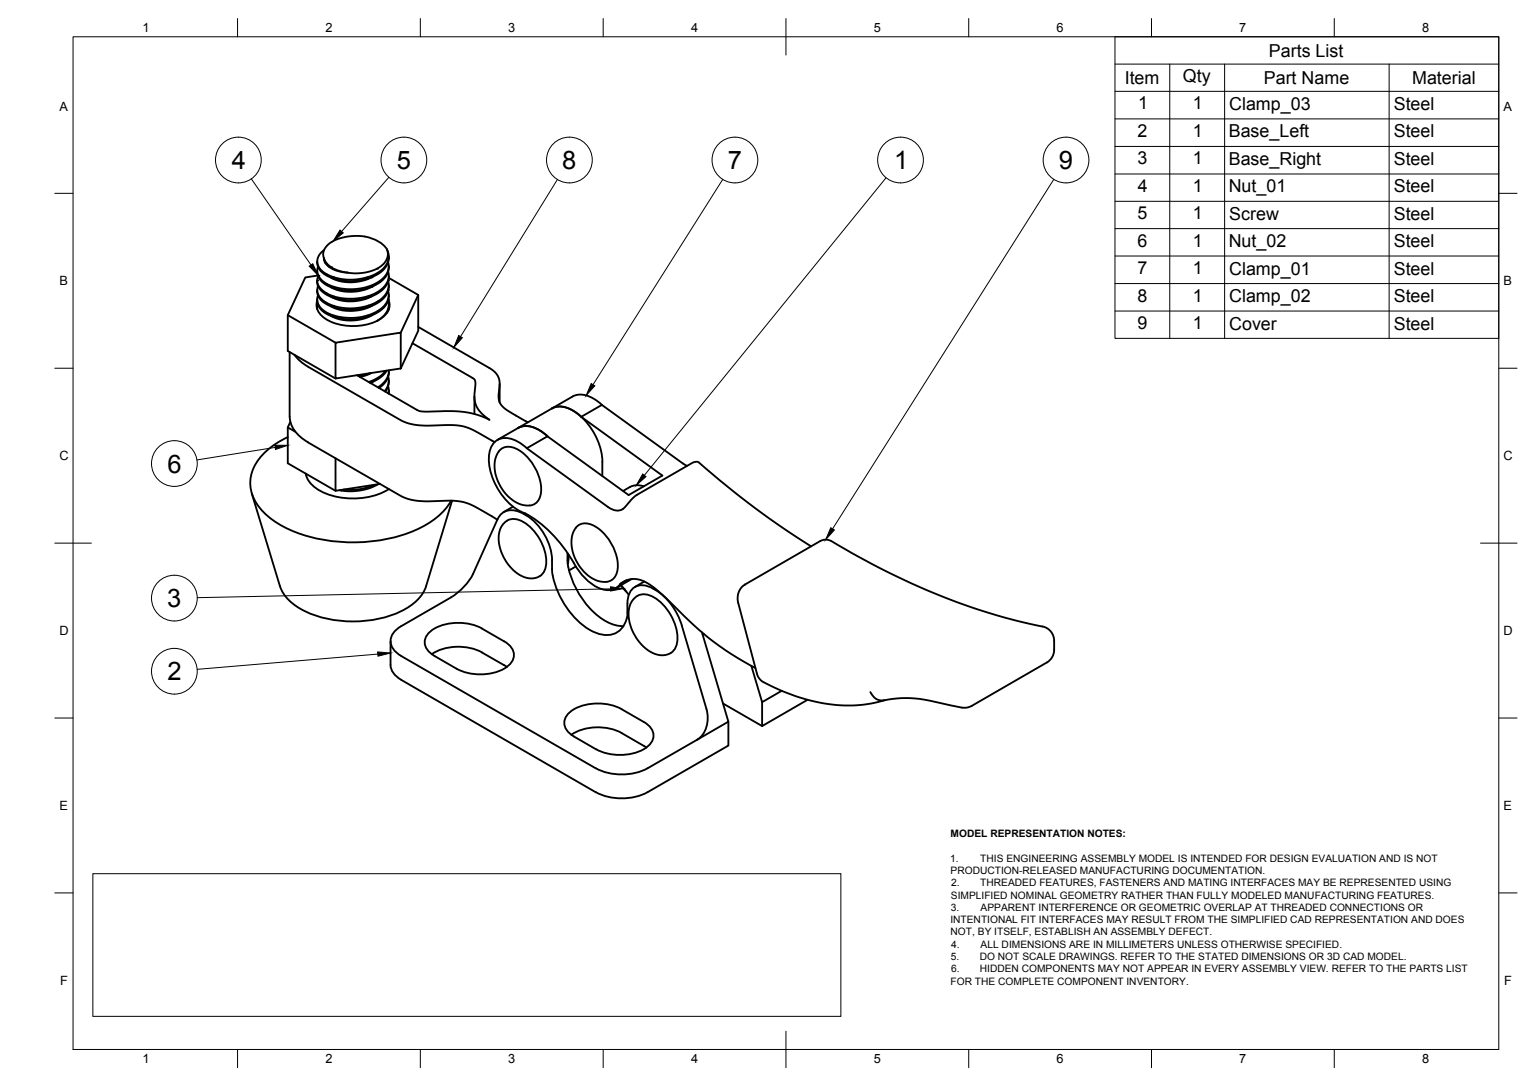
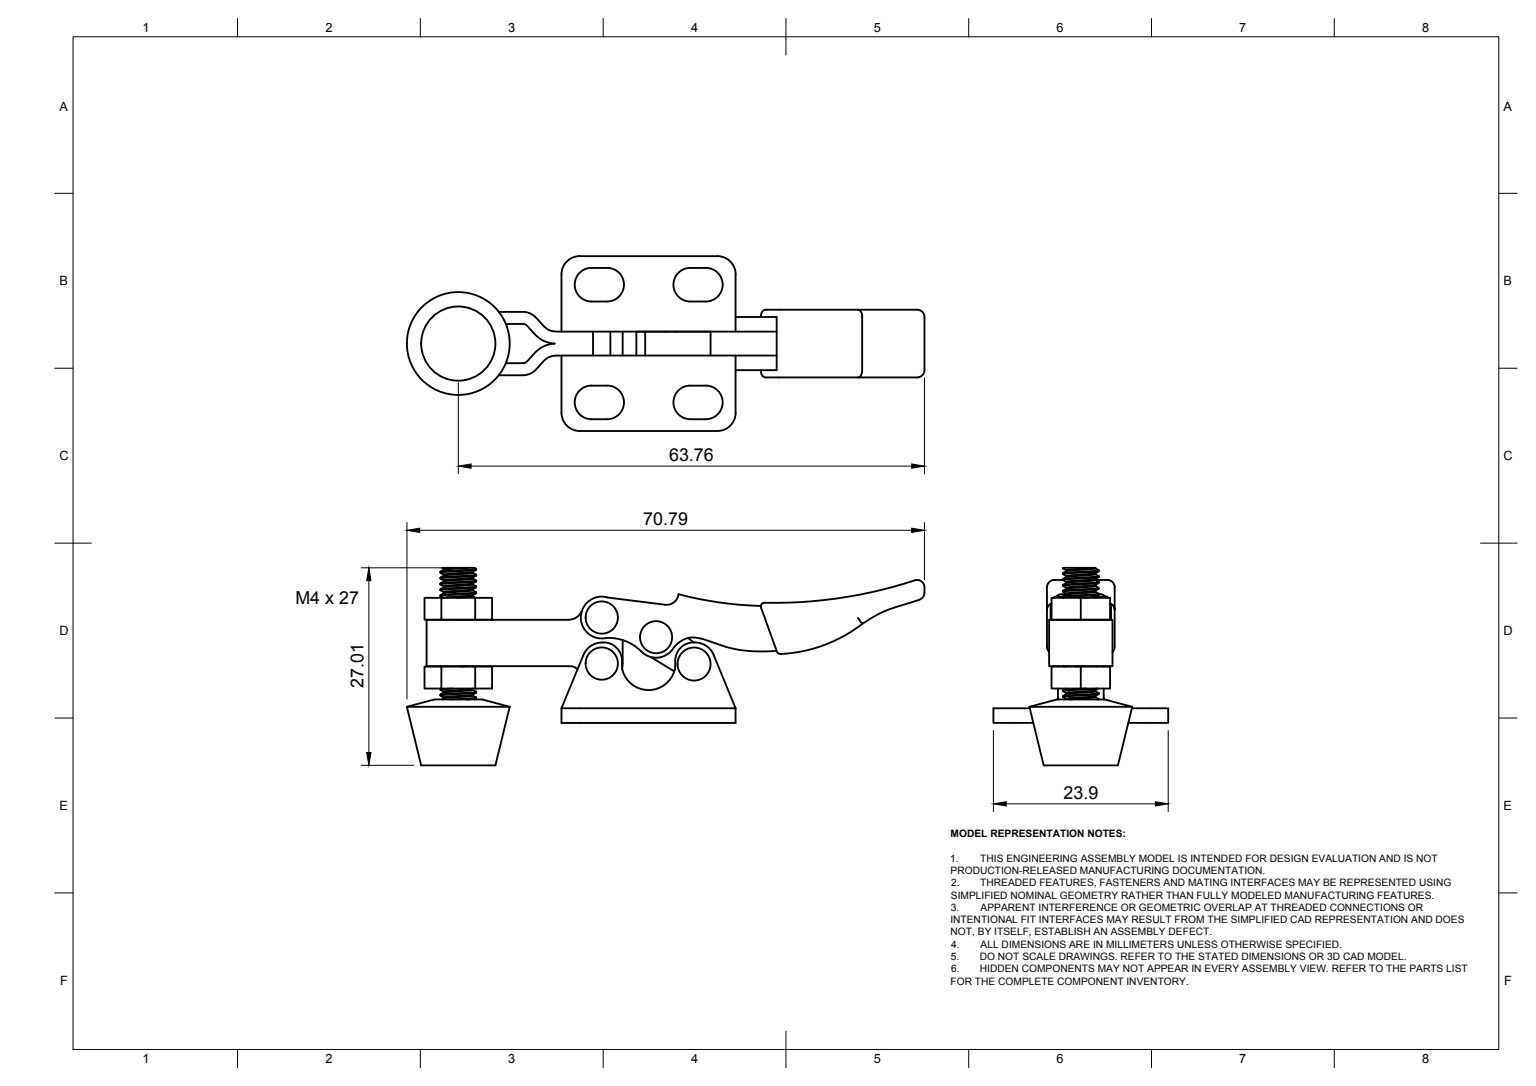
ISO-10303-21;
HEADER;
/* Generated by software containing ST-Developer
 * from STEP Tools, Inc. (www.steptools.com) 
 */

FILE_DESCRIPTION(
/* description */ (''),
/* implementation_level */ '2;1');

FILE_NAME(
/* name */ 'BR-203',
/* time_stamp */ '2026-10-05T16:20:14-07:00',
/* author */ (''),
/* organization */ (''),
/* preprocessor_version */ 'ST-DEVELOPER v20.2',
/* originating_system */ 'Autodesk Translation Framework v15.15.0.0',
/* authorisation */ '');

FILE_SCHEMA (('AUTOMOTIVE_DESIGN { 1 0 10303 214 3 1 1 }'));
ENDSEC;

DATA;
#10=MECHANICAL_DESIGN_GEOMETRIC_PRESENTATION_REPRESENTATION('',(#247,#248,
#249,#250,#251,#252,#253,#254,#255),#23577);
#11=ITEM_DEFINED_TRANSFORMATION($,$,#4267,#4665);
#12=ITEM_DEFINED_TRANSFORMATION($,$,#4284,#4666);
#13=ITEM_DEFINED_TRANSFORMATION($,$,#4354,#4667);
#14=ITEM_DEFINED_TRANSFORMATION($,$,#4424,#4668);
#15=ITEM_DEFINED_TRANSFORMATION($,$,#4436,#4669);
#16=ITEM_DEFINED_TRANSFORMATION($,$,#4473,#4670);
#17=ITEM_DEFINED_TRANSFORMATION($,$,#4485,#4671);
#18=ITEM_DEFINED_TRANSFORMATION($,$,#4573,#4672);
#19=ITEM_DEFINED_TRANSFORMATION($,$,#4607,#4673);
#20=(
REPRESENTATION_RELATIONSHIP($,$,#23612,#23611)
REPRESENTATION_RELATIONSHIP_WITH_TRANSFORMATION(#11)
SHAPE_REPRESENTATION_RELATIONSHIP()
);
#21=(
REPRESENTATION_RELATIONSHIP($,$,#23613,#23611)
REPRESENTATION_RELATIONSHIP_WITH_TRANSFORMATION(#12)
SHAPE_REPRESENTATION_RELATIONSHIP()
);
#22=(
REPRESENTATION_RELATIONSHIP($,$,#23614,#23611)
REPRESENTATION_RELATIONSHIP_WITH_TRANSFORMATION(#13)
SHAPE_REPRESENTATION_RELATIONSHIP()
);
#23=(
REPRESENTATION_RELATIONSHIP($,$,#23615,#23611)
REPRESENTATION_RELATIONSHIP_WITH_TRANSFORMATION(#14)
SHAPE_REPRESENTATION_RELATIONSHIP()
);
#24=(
REPRESENTATION_RELATIONSHIP($,$,#23616,#23611)
REPRESENTATION_RELATIONSHIP_WITH_TRANSFORMATION(#15)
SHAPE_REPRESENTATION_RELATIONSHIP()
);
#25=(
REPRESENTATION_RELATIONSHIP($,$,#23617,#23611)
REPRESENTATION_RELATIONSHIP_WITH_TRANSFORMATION(#16)
SHAPE_REPRESENTATION_RELATIONSHIP()
);
#26=(
REPRESENTATION_RELATIONSHIP($,$,#23618,#23611)
REPRESENTATION_RELATIONSHIP_WITH_TRANSFORMATION(#17)
SHAPE_REPRESENTATION_RELATIONSHIP()
);
#27=(
REPRESENTATION_RELATIONSHIP($,$,#23619,#23611)
REPRESENTATION_RELATIONSHIP_WITH_TRANSFORMATION(#18)
SHAPE_REPRESENTATION_RELATIONSHIP()
);
#28=(
REPRESENTATION_RELATIONSHIP($,$,#23620,#23611)
REPRESENTATION_RELATIONSHIP_WITH_TRANSFORMATION(#19)
SHAPE_REPRESENTATION_RELATIONSHIP()
);
#29=CONTEXT_DEPENDENT_SHAPE_REPRESENTATION(#20,#23602);
#30=CONTEXT_DEPENDENT_SHAPE_REPRESENTATION(#21,#23603);
#31=CONTEXT_DEPENDENT_SHAPE_REPRESENTATION(#22,#23604);
#32=CONTEXT_DEPENDENT_SHAPE_REPRESENTATION(#23,#23605);
#33=CONTEXT_DEPENDENT_SHAPE_REPRESENTATION(#24,#23606);
#34=CONTEXT_DEPENDENT_SHAPE_REPRESENTATION(#25,#23607);
#35=CONTEXT_DEPENDENT_SHAPE_REPRESENTATION(#26,#23608);
#36=CONTEXT_DEPENDENT_SHAPE_REPRESENTATION(#27,#23609);
#37=CONTEXT_DEPENDENT_SHAPE_REPRESENTATION(#28,#23610);
#38=NEXT_ASSEMBLY_USAGE_OCCURRENCE('Clamp_03:1','Clamp_03:1',
'Clamp_03:1',#23622,#23623,'Clamp_03:1');
#39=NEXT_ASSEMBLY_USAGE_OCCURRENCE('Base_Left:1','Base_Left:1',
'Base_Left:1',#23622,#23624,'Base_Left:1');
#40=NEXT_ASSEMBLY_USAGE_OCCURRENCE('Base_Right:1','Base_Right:1',
'Base_Right:1',#23622,#23625,'Base_Right:1');
#41=NEXT_ASSEMBLY_USAGE_OCCURRENCE('Nut_01:1','Nut_01:1','Nut_01:1',#23622,
#23626,'Nut_01:1');
#42=NEXT_ASSEMBLY_USAGE_OCCURRENCE('Screw:1','Screw:1','Screw:1',#23622,
#23627,'Screw:1');
#43=NEXT_ASSEMBLY_USAGE_OCCURRENCE('Nut_02:1','Nut_02:1','Nut_02:1',#23622,
#23628,'Nut_02:1');
#44=NEXT_ASSEMBLY_USAGE_OCCURRENCE('Clamp_01:1','Clamp_01:1',
'Clamp_01:1',#23622,#23629,'Clamp_01:1');
#45=NEXT_ASSEMBLY_USAGE_OCCURRENCE('Clamp_02:1','Clamp_02:1',
'Clamp_02:1',#23622,#23630,'Clamp_02:1');
#46=NEXT_ASSEMBLY_USAGE_OCCURRENCE('Cover:1','Cover:1','Cover:1',#23622,
#23631,'Cover:1');
#47=SPHERICAL_SURFACE('',#4635,1.);
#48=SPHERICAL_SURFACE('',#4644,1.);
#49=SPHERICAL_SURFACE('',#4650,1.);
#50=SPHERICAL_SURFACE('',#4654,1.);
#51=CONICAL_SURFACE('',#4468,5.14028464662889,1.31156275926766);
#52=CONICAL_SURFACE('',#4470,6.05319927020769,0.239535482048054);
#53=B_SPLINE_SURFACE_WITH_KNOTS('',3,3,((#19950,#19951,#19952,#19953,#19954,
#19955,#19956,#19957,#19958,#19959,#19960,#19961,#19962,#19963,#19964,#19965,
#19966,#19967,#19968,#19969,#19970,#19971,#19972,#19973,#19974,#19975,#19976,
#19977,#19978,#19979,#19980,#19981,#19982,#19983,#19984,#19985,#19986,#19987,
#19988,#19989,#19990,#19991,#19992,#19993,#19994,#19995,#19996,#19997,#19998,
#19999,#20000,#20001,#20002,#20003,#20004,#20005,#20006,#20007,#20008,#20009,
#20010,#20011,#20012,#20013,#20014,#20015,#20016,#20017,#20018,#20019,#20020,
#20021,#20022,#20023,#20024,#20025,#20026,#20027,#20028,#20029,#20030,#20031,
#20032,#20033,#20034,#20035,#20036,#20037,#20038,#20039,#20040,#20041,#20042,
#20043,#20044,#20045,#20046,#20047,#20048,#20049,#20050,#20051,#20052,#20053,
#20054,#20055,#20056,#20057,#20058,#20059,#20060,#20061,#20062,#20063,#20064,
#20065,#20066,#20067,#20068,#20069,#20070,#20071,#20072,#20073,#20074,#20075,
#20076,#20077,#20078,#20079,#20080,#20081,#20082,#20083,#20084,#20085,#20086,
#20087,#20088,#20089,#20090,#20091,#20092,#20093,#20094,#20095,#20096),
(#20097,#20098,#20099,#20100,#20101,#20102,#20103,#20104,#20105,#20106,
#20107,#20108,#20109,#20110,#20111,#20112,#20113,#20114,#20115,#20116,#20117,
#20118,#20119,#20120,#20121,#20122,#20123,#20124,#20125,#20126,#20127,#20128,
#20129,#20130,#20131,#20132,#20133,#20134,#20135,#20136,#20137,#20138,#20139,
#20140,#20141,#20142,#20143,#20144,#20145,#20146,#20147,#20148,#20149,#20150,
#20151,#20152,#20153,#20154,#20155,#20156,#20157,#20158,#20159,#20160,#20161,
#20162,#20163,#20164,#20165,#20166,#20167,#20168,#20169,#20170,#20171,#20172,
#20173,#20174,#20175,#20176,#20177,#20178,#20179,#20180,#20181,#20182,#20183,
#20184,#20185,#20186,#20187,#20188,#20189,#20190,#20191,#20192,#20193,#20194,
#20195,#20196,#20197,#20198,#20199,#20200,#20201,#20202,#20203,#20204,#20205,
#20206,#20207,#20208,#20209,#20210,#20211,#20212,#20213,#20214,#20215,#20216,
#20217,#20218,#20219,#20220,#20221,#20222,#20223,#20224,#20225,#20226,#20227,
#20228,#20229,#20230,#20231,#20232,#20233,#20234,#20235,#20236,#20237,#20238,
#20239,#20240,#20241,#20242,#20243),(#20244,#20245,#20246,#20247,#20248,
#20249,#20250,#20251,#20252,#20253,#20254,#20255,#20256,#20257,#20258,#20259,
#20260,#20261,#20262,#20263,#20264,#20265,#20266,#20267,#20268,#20269,#20270,
#20271,#20272,#20273,#20274,#20275,#20276,#20277,#20278,#20279,#20280,#20281,
#20282,#20283,#20284,#20285,#20286,#20287,#20288,#20289,#20290,#20291,#20292,
#20293,#20294,#20295,#20296,#20297,#20298,#20299,#20300,#20301,#20302,#20303,
#20304,#20305,#20306,#20307,#20308,#20309,#20310,#20311,#20312,#20313,#20314,
#20315,#20316,#20317,#20318,#20319,#20320,#20321,#20322,#20323,#20324,#20325,
#20326,#20327,#20328,#20329,#20330,#20331,#20332,#20333,#20334,#20335,#20336,
#20337,#20338,#20339,#20340,#20341,#20342,#20343,#20344,#20345,#20346,#20347,
#20348,#20349,#20350,#20351,#20352,#20353,#20354,#20355,#20356,#20357,#20358,
#20359,#20360,#20361,#20362,#20363,#20364,#20365,#20366,#20367,#20368,#20369,
#20370,#20371,#20372,#20373,#20374,#20375,#20376,#20377,#20378,#20379,#20380,
#20381,#20382,#20383,#20384,#20385,#20386,#20387,#20388,#20389,#20390),
(#20391,#20392,#20393,#20394,#20395,#20396,#20397,#20398,#20399,#20400,
#20401,#20402,#20403,#20404,#20405,#20406,#20407,#20408,#20409,#20410,#20411,
#20412,#20413,#20414,#20415,#20416,#20417,#20418,#20419,#20420,#20421,#20422,
#20423,#20424,#20425,#20426,#20427,#20428,#20429,#20430,#20431,#20432,#20433,
#20434,#20435,#20436,#20437,#20438,#20439,#20440,#20441,#20442,#20443,#20444,
#20445,#20446,#20447,#20448,#20449,#20450,#20451,#20452,#20453,#20454,#20455,
#20456,#20457,#20458,#20459,#20460,#20461,#20462,#20463,#20464,#20465,#20466,
#20467,#20468,#20469,#20470,#20471,#20472,#20473,#20474,#20475,#20476,#20477,
#20478,#20479,#20480,#20481,#20482,#20483,#20484,#20485,#20486,#20487,#20488,
#20489,#20490,#20491,#20492,#20493,#20494,#20495,#20496,#20497,#20498,#20499,
#20500,#20501,#20502,#20503,#20504,#20505,#20506,#20507,#20508,#20509,#20510,
#20511,#20512,#20513,#20514,#20515,#20516,#20517,#20518,#20519,#20520,#20521,
#20522,#20523,#20524,#20525,#20526,#20527,#20528,#20529,#20530,#20531,#20532,
#20533,#20534,#20535,#20536,#20537)),.UNSPECIFIED.,.F.,.F.,.F.,(4,4),(4,
1,1,1,1,1,1,1,1,1,1,1,1,1,1,1,1,1,1,1,1,1,1,1,1,1,1,1,1,1,1,1,1,1,1,1,1,
1,1,1,1,1,1,1,1,1,1,1,1,1,1,1,1,1,1,1,1,1,1,1,1,1,1,1,1,1,1,1,1,1,1,1,1,
1,1,1,1,1,1,1,1,1,1,1,1,1,1,1,1,1,1,1,1,1,1,1,1,1,1,1,1,1,1,1,1,1,1,1,1,
1,1,1,1,1,1,1,1,1,1,1,1,1,1,1,1,1,1,1,1,1,1,1,1,1,1,1,1,1,1,1,1,1,1,1,4),
(-0.000407634560164902,0.0529903850324167),(8.30815772716265,9.30425680398324,
10.3003558808038,11.2964549576244,12.292554034445,13.2886531112656,14.2847521880862,
15.2808512649068,16.2769503417274,17.273049418548,18.2691484953686,19.2652475721892,
20.2613466490097,21.2574457258303,22.2535448026509,23.2496438794715,24.2457429562921,
25.2418420331127,26.2379411099333,27.2340401867539,28.2301392635745,29.2262383403951,
30.2223374172156,31.2184364940362,32.2145355708568,33.2106346476774,34.206733724498,
35.2028328013186,36.1989318781392,37.1950309549598,38.1911300317804,39.187229108601,
40.1833281854216,41.1794272622421,42.1755263390627,43.1716254158833,44.1677244927039,
45.1638235695245,46.1599226463451,47.1560217231657,48.1521207999863,49.1482198768069,
50.1443189536275,51.1404180304481,52.1365171072686,53.1326161840892,54.1287152609098,
55.1248143377304,56.120913414551,57.1170124913716,58.1131115681922,59.1092106450128,
60.1053097218334,61.101408798654,62.0975078754745,63.0936069522951,64.0897060291157,
65.0858051059363,66.0819041827569,67.0780032595775,68.0741023363981,69.0702014132187,
70.0663004900393,71.0623995668599,72.0584986436805,73.0545977205011,74.0506967973216,
75.0467958741422,76.0428949509628,77.0389940277834,78.035093104604,79.0311921814246,
80.0272912582452,81.0233903350658,82.0194894118864,83.015588488707,84.0116875655276,
85.0077866423481,86.0038857191687,86.9999847959893,87.9960838728099,88.9921829496305,
89.9882820264511,90.9843811032717,91.9804801800923,92.9765792569129,93.9726783337335,
94.968777410554,95.9648764873746,96.9609755641952,97.9570746410158,98.9531737178364,
99.949272794657,100.945371871478,101.941470948298,102.937570025119,103.933669101939,
104.92976817876,105.925867255581,106.921966332401,107.918065409222,108.914164486042,
109.910263562863,110.906362639683,111.902461716504,112.898560793325,113.894659870145,
114.890758946966,115.886858023786,116.882957100607,117.879056177428,118.875155254248,
119.871254331069,120.867353407889,121.86345248471,122.859551561531,123.855650638351,
124.851749715172,125.847848791992,126.843947868813,127.840046945634,128.836146022454,
129.832245099275,130.828344176095,131.824443252916,132.820542329736,133.816641406557,
134.812740483378,135.808839560198,136.804938637019,137.801037713839,138.79713679066,
139.793235867481,140.789334944301,141.785434021122,142.781533097942,143.777632174763,
144.773731251584,145.769830328404,146.765929405225,147.762028482045,148.758127558866,
149.754226635687,150.750325712507,151.746832423888),.UNSPECIFIED.);
#54=B_SPLINE_SURFACE_WITH_KNOTS('',3,3,((#20716,#20717,#20718,#20719,#20720,
#20721,#20722,#20723,#20724,#20725,#20726,#20727,#20728,#20729,#20730,#20731,
#20732,#20733,#20734,#20735,#20736,#20737,#20738,#20739,#20740,#20741,#20742,
#20743,#20744,#20745,#20746,#20747,#20748,#20749,#20750,#20751,#20752,#20753,
#20754,#20755,#20756,#20757,#20758,#20759,#20760,#20761,#20762,#20763,#20764,
#20765,#20766,#20767,#20768,#20769,#20770,#20771,#20772,#20773,#20774,#20775,
#20776,#20777,#20778,#20779,#20780,#20781,#20782,#20783,#20784,#20785,#20786,
#20787,#20788,#20789,#20790,#20791,#20792,#20793,#20794,#20795,#20796,#20797,
#20798,#20799,#20800,#20801,#20802,#20803,#20804,#20805,#20806,#20807,#20808,
#20809,#20810,#20811,#20812,#20813,#20814,#20815,#20816,#20817,#20818,#20819,
#20820,#20821,#20822,#20823,#20824,#20825,#20826,#20827,#20828,#20829,#20830,
#20831,#20832,#20833,#20834,#20835,#20836,#20837,#20838,#20839,#20840,#20841,
#20842,#20843,#20844,#20845,#20846,#20847,#20848,#20849,#20850,#20851,#20852,
#20853,#20854,#20855,#20856,#20857,#20858,#20859,#20860,#20861,#20862),
(#20863,#20864,#20865,#20866,#20867,#20868,#20869,#20870,#20871,#20872,
#20873,#20874,#20875,#20876,#20877,#20878,#20879,#20880,#20881,#20882,#20883,
#20884,#20885,#20886,#20887,#20888,#20889,#20890,#20891,#20892,#20893,#20894,
#20895,#20896,#20897,#20898,#20899,#20900,#20901,#20902,#20903,#20904,#20905,
#20906,#20907,#20908,#20909,#20910,#20911,#20912,#20913,#20914,#20915,#20916,
#20917,#20918,#20919,#20920,#20921,#20922,#20923,#20924,#20925,#20926,#20927,
#20928,#20929,#20930,#20931,#20932,#20933,#20934,#20935,#20936,#20937,#20938,
#20939,#20940,#20941,#20942,#20943,#20944,#20945,#20946,#20947,#20948,#20949,
#20950,#20951,#20952,#20953,#20954,#20955,#20956,#20957,#20958,#20959,#20960,
#20961,#20962,#20963,#20964,#20965,#20966,#20967,#20968,#20969,#20970,#20971,
#20972,#20973,#20974,#20975,#20976,#20977,#20978,#20979,#20980,#20981,#20982,
#20983,#20984,#20985,#20986,#20987,#20988,#20989,#20990,#20991,#20992,#20993,
#20994,#20995,#20996,#20997,#20998,#20999,#21000,#21001,#21002,#21003,#21004,
#21005,#21006,#21007,#21008,#21009),(#21010,#21011,#21012,#21013,#21014,
#21015,#21016,#21017,#21018,#21019,#21020,#21021,#21022,#21023,#21024,#21025,
#21026,#21027,#21028,#21029,#21030,#21031,#21032,#21033,#21034,#21035,#21036,
#21037,#21038,#21039,#21040,#21041,#21042,#21043,#21044,#21045,#21046,#21047,
#21048,#21049,#21050,#21051,#21052,#21053,#21054,#21055,#21056,#21057,#21058,
#21059,#21060,#21061,#21062,#21063,#21064,#21065,#21066,#21067,#21068,#21069,
#21070,#21071,#21072,#21073,#21074,#21075,#21076,#21077,#21078,#21079,#21080,
#21081,#21082,#21083,#21084,#21085,#21086,#21087,#21088,#21089,#21090,#21091,
#21092,#21093,#21094,#21095,#21096,#21097,#21098,#21099,#21100,#21101,#21102,
#21103,#21104,#21105,#21106,#21107,#21108,#21109,#21110,#21111,#21112,#21113,
#21114,#21115,#21116,#21117,#21118,#21119,#21120,#21121,#21122,#21123,#21124,
#21125,#21126,#21127,#21128,#21129,#21130,#21131,#21132,#21133,#21134,#21135,
#21136,#21137,#21138,#21139,#21140,#21141,#21142,#21143,#21144,#21145,#21146,
#21147,#21148,#21149,#21150,#21151,#21152,#21153,#21154,#21155,#21156),
(#21157,#21158,#21159,#21160,#21161,#21162,#21163,#21164,#21165,#21166,
#21167,#21168,#21169,#21170,#21171,#21172,#21173,#21174,#21175,#21176,#21177,
#21178,#21179,#21180,#21181,#21182,#21183,#21184,#21185,#21186,#21187,#21188,
#21189,#21190,#21191,#21192,#21193,#21194,#21195,#21196,#21197,#21198,#21199,
#21200,#21201,#21202,#21203,#21204,#21205,#21206,#21207,#21208,#21209,#21210,
#21211,#21212,#21213,#21214,#21215,#21216,#21217,#21218,#21219,#21220,#21221,
#21222,#21223,#21224,#21225,#21226,#21227,#21228,#21229,#21230,#21231,#21232,
#21233,#21234,#21235,#21236,#21237,#21238,#21239,#21240,#21241,#21242,#21243,
#21244,#21245,#21246,#21247,#21248,#21249,#21250,#21251,#21252,#21253,#21254,
#21255,#21256,#21257,#21258,#21259,#21260,#21261,#21262,#21263,#21264,#21265,
#21266,#21267,#21268,#21269,#21270,#21271,#21272,#21273,#21274,#21275,#21276,
#21277,#21278,#21279,#21280,#21281,#21282,#21283,#21284,#21285,#21286,#21287,
#21288,#21289,#21290,#21291,#21292,#21293,#21294,#21295,#21296,#21297,#21298,
#21299,#21300,#21301,#21302,#21303)),.UNSPECIFIED.,.F.,.F.,.F.,(4,4),(4,
1,1,1,1,1,1,1,1,1,1,1,1,1,1,1,1,1,1,1,1,1,1,1,1,1,1,1,1,1,1,1,1,1,1,1,1,
1,1,1,1,1,1,1,1,1,1,1,1,1,1,1,1,1,1,1,1,1,1,1,1,1,1,1,1,1,1,1,1,1,1,1,1,
1,1,1,1,1,1,1,1,1,1,1,1,1,1,1,1,1,1,1,1,1,1,1,1,1,1,1,1,1,1,1,1,1,1,1,1,
1,1,1,1,1,1,1,1,1,1,1,1,1,1,1,1,1,1,1,1,1,1,1,1,1,1,1,1,1,1,1,1,1,1,1,4),
(-0.000364909195550823,0.0530331194684996),(11.6159855549096,12.6124922741621,
13.6085913509826,14.6046904278032,15.6007895046238,16.5968885814444,17.592987658265,
18.5890867350856,19.5851858119062,20.5812848887268,21.5773839655474,22.573483042368,
23.5695821191886,24.5656811960091,25.5617802728297,26.5578793496503,27.5539784264709,
28.5500775032915,29.5461765801121,30.5422756569327,31.5383747337533,32.5344738105739,
33.5305728873945,34.5266719642151,35.5227710410356,36.5188701178562,37.5149691946768,
38.5110682714974,39.507167348318,40.5032664251386,41.4993655019592,42.4954645787798,
43.4915636556004,44.487662732421,45.4837618092415,46.4798608860621,47.4759599628827,
48.4720590397033,49.4681581165239,50.4642571933445,51.4603562701651,52.4564553469857,
53.4525544238063,54.4486535006269,55.4447525774475,56.4408516542681,57.4369507310886,
58.4330498079092,59.4291488847298,60.4252479615504,61.421347038371,62.4174461151916,
63.4135451920122,64.4096442688328,65.4057433456534,66.4018424224739,67.3979414992945,
68.3940405761151,69.3901396529357,70.3862387297563,71.3823378065769,72.3784368833975,
73.3745359602181,74.3706350370387,75.3667341138593,76.3628331906799,77.3589322675004,
78.355031344321,79.3511304211416,80.3472294979622,81.3433285747828,82.3394276516034,
83.335526728424,84.3316258052446,85.3277248820652,86.3238239588858,87.3199230357064,
88.316022112527,89.3121211893476,90.3082202661681,91.3043193429887,92.3004184198093,
93.2965174966299,94.2926165734505,95.2887156502711,96.2848147270917,97.2809138039123,
98.2770128807329,99.2731119575535,100.269211034374,101.265310111195,102.261409188015,
103.257508264836,104.253607341656,105.249706418477,106.245805495298,107.241904572118,
108.238003648939,109.234102725759,110.23020180258,111.226300879401,112.222399956221,
113.218499033042,114.214598109862,115.210697186683,116.206796263503,117.202895340324,
118.198994417145,119.195093493965,120.191192570786,121.187291647606,122.183390724427,
123.179489801248,124.175588878068,125.171687954889,126.167787031709,127.16388610853,
128.159985185351,129.156084262171,130.152183338992,131.148282415812,132.144381492633,
133.140480569454,134.136579646274,135.132678723095,136.128777799915,137.124876876736,
138.120975953556,139.117075030377,140.113174107198,141.109273184018,142.105372260839,
143.101471337659,144.09757041448,145.093669491301,146.089768568121,147.085867644942,
148.081966721762,149.078065798583,150.074164875404,151.070263952224,152.066363029045,
153.062462105865,154.058561182686,155.054660259507),.UNSPECIFIED.);
#55=B_SPLINE_SURFACE_WITH_KNOTS('',5,1,((#21755,#21756),(#21757,#21758),
(#21759,#21760),(#21761,#21762),(#21763,#21764),(#21765,#21766),(#21767,
#21768),(#21769,#21770),(#21771,#21772),(#21773,#21774),(#21775,#21776),
(#21777,#21778),(#21779,#21780),(#21781,#21782),(#21783,#21784),(#21785,
#21786),(#21787,#21788),(#21789,#21790),(#21791,#21792),(#21793,#21794),
(#21795,#21796),(#21797,#21798),(#21799,#21800),(#21801,#21802),(#21803,
#21804),(#21805,#21806),(#21807,#21808),(#21809,#21810),(#21811,#21812),
(#21813,#21814),(#21815,#21816),(#21817,#21818),(#21819,#21820),(#21821,
#21822),(#21823,#21824),(#21825,#21826),(#21827,#21828),(#21829,#21830),
(#21831,#21832),(#21833,#21834),(#21835,#21836),(#21837,#21838),(#21839,
#21840),(#21841,#21842),(#21843,#21844),(#21845,#21846),(#21847,#21848),
(#21849,#21850),(#21851,#21852),(#21853,#21854),(#21855,#21856),(#21857,
#21858),(#21859,#21860),(#21861,#21862),(#21863,#21864)),.UNSPECIFIED.,
 .F.,.F.,.F.,(6,1,1,1,1,1,1,1,1,1,1,1,1,1,1,1,1,1,1,1,1,1,1,1,1,1,1,1,1,
1,1,1,1,1,1,1,1,1,1,1,1,1,1,1,1,1,1,1,1,1,6),(2,2),(0.,0.02,0.04,0.06,0.08,
0.1,0.12,0.14,0.16,0.18,0.2,0.22,0.24,0.26,0.28,0.3,0.32,0.34,0.36,0.38,
0.4,0.42,0.44,0.46,0.48,0.5,0.52,0.54,0.56,0.58,0.6,0.62,0.64,0.66,0.68,
0.7,0.72,0.74,0.76,0.78,0.8,0.82,0.84,0.86,0.88,0.9,0.92,0.940000000000001,
0.960000000000001,0.980000000000001,0.99866513431215),(0.,0.24),
 .UNSPECIFIED.);
#56=B_SPLINE_SURFACE_WITH_KNOTS('',5,1,((#22096,#22097),(#22098,#22099),
(#22100,#22101),(#22102,#22103),(#22104,#22105),(#22106,#22107),(#22108,
#22109),(#22110,#22111),(#22112,#22113),(#22114,#22115),(#22116,#22117),
(#22118,#22119),(#22120,#22121),(#22122,#22123),(#22124,#22125),(#22126,
#22127),(#22128,#22129),(#22130,#22131),(#22132,#22133),(#22134,#22135),
(#22136,#22137),(#22138,#22139),(#22140,#22141),(#22142,#22143),(#22144,
#22145),(#22146,#22147),(#22148,#22149),(#22150,#22151),(#22152,#22153),
(#22154,#22155),(#22156,#22157),(#22158,#22159),(#22160,#22161),(#22162,
#22163),(#22164,#22165),(#22166,#22167),(#22168,#22169),(#22170,#22171),
(#22172,#22173),(#22174,#22175),(#22176,#22177),(#22178,#22179),(#22180,
#22181),(#22182,#22183),(#22184,#22185),(#22186,#22187),(#22188,#22189),
(#22190,#22191),(#22192,#22193),(#22194,#22195),(#22196,#22197),(#22198,
#22199),(#22200,#22201),(#22202,#22203),(#22204,#22205)),.UNSPECIFIED.,
 .F.,.F.,.F.,(6,1,1,1,1,1,1,1,1,1,1,1,1,1,1,1,1,1,1,1,1,1,1,1,1,1,1,1,1,
1,1,1,1,1,1,1,1,1,1,1,1,1,1,1,1,1,1,1,1,1,6),(2,2),(0.,0.02,0.04,0.06,0.08,
0.1,0.12,0.14,0.16,0.18,0.2,0.22,0.24,0.26,0.28,0.3,0.32,0.34,0.36,0.38,
0.4,0.42,0.44,0.46,0.48,0.5,0.52,0.54,0.56,0.58,0.6,0.62,0.64,0.66,0.68,
0.7,0.72,0.74,0.76,0.78,0.8,0.82,0.84,0.86,0.88,0.9,0.92,0.940000000000001,
0.960000000000001,0.980000000000001,0.99866513431215),(0.,0.24),
 .UNSPECIFIED.);
#57=B_SPLINE_SURFACE_WITH_KNOTS('',5,1,((#22213,#22214),(#22215,#22216),
(#22217,#22218),(#22219,#22220),(#22221,#22222),(#22223,#22224),(#22225,
#22226),(#22227,#22228),(#22229,#22230),(#22231,#22232),(#22233,#22234),
(#22235,#22236),(#22237,#22238),(#22239,#22240),(#22241,#22242),(#22243,
#22244),(#22245,#22246),(#22247,#22248),(#22249,#22250),(#22251,#22252)),
 .UNSPECIFIED.,.F.,.F.,.F.,(6,1,1,1,1,1,1,1,1,1,1,1,1,1,1,6),(2,2),(0.,
0.0666666666666667,0.133333333333333,0.2,0.266666666666667,0.333333333333333,
0.4,0.466666666666667,0.533333333333333,0.6,0.666666666666667,0.733333333333333,
0.8,0.866666666666667,0.933333333333333,1.),(0.,1.44),.UNSPECIFIED.);
#58=B_SPLINE_SURFACE_WITH_KNOTS('',3,1,((#22299,#22300),(#22301,#22302),
(#22303,#22304),(#22305,#22306),(#22307,#22308),(#22309,#22310),(#22311,
#22312),(#22313,#22314),(#22315,#22316),(#22317,#22318),(#22319,#22320),
(#22321,#22322),(#22323,#22324),(#22325,#22326),(#22327,#22328),(#22329,
#22330)),.UNSPECIFIED.,.F.,.F.,.F.,(4,3,3,3,3,4),(2,2),(-1.,-0.857074929962035,
-0.680580226328136,-0.49099360586306,-0.247446976985656,0.),(0.,1.44229698166468),
 .UNSPECIFIED.);
#59=B_SPLINE_SURFACE_WITH_KNOTS('',3,1,((#22422,#22423),(#22424,#22425),
(#22426,#22427),(#22428,#22429),(#22430,#22431),(#22432,#22433),(#22434,
#22435),(#22436,#22437),(#22438,#22439),(#22440,#22441),(#22442,#22443),
(#22444,#22445),(#22446,#22447),(#22448,#22449),(#22450,#22451),(#22452,
#22453)),.UNSPECIFIED.,.F.,.F.,.F.,(4,3,3,3,3,4),(2,2),(-1.,-0.857074929962035,
-0.680580226328136,-0.49099360586306,-0.247446976985656,0.),(0.,1.44229698166468),
 .UNSPECIFIED.);
#60=B_SPLINE_SURFACE_WITH_KNOTS('',5,1,((#22519,#22520),(#22521,#22522),
(#22523,#22524),(#22525,#22526),(#22527,#22528),(#22529,#22530),(#22531,
#22532),(#22533,#22534),(#22535,#22536),(#22537,#22538),(#22539,#22540),
(#22541,#22542),(#22543,#22544),(#22545,#22546),(#22547,#22548),(#22549,
#22550),(#22551,#22552),(#22553,#22554),(#22555,#22556),(#22557,#22558)),
 .UNSPECIFIED.,.F.,.F.,.F.,(6,1,1,1,1,1,1,1,1,1,1,1,1,1,1,6),(2,2),(0.,
0.0666666666666667,0.133333333333333,0.2,0.266666666666667,0.333333333333333,
0.4,0.466666666666667,0.533333333333333,0.6,0.666666666666667,0.733333333333333,
0.8,0.866666666666667,0.933333333333333,1.),(0.,2.88),.UNSPECIFIED.);
#61=B_SPLINE_SURFACE_WITH_KNOTS('',5,1,((#22641,#22642),(#22643,#22644),
(#22645,#22646),(#22647,#22648),(#22649,#22650),(#22651,#22652),(#22653,
#22654),(#22655,#22656),(#22657,#22658),(#22659,#22660),(#22661,#22662),
(#22663,#22664),(#22665,#22666),(#22667,#22668),(#22669,#22670),(#22671,
#22672),(#22673,#22674),(#22675,#22676),(#22677,#22678),(#22679,#22680)),
 .UNSPECIFIED.,.F.,.F.,.F.,(6,1,1,1,1,1,1,1,1,1,1,1,1,1,1,6),(2,2),(0.,
0.0666666666666667,0.133333333333333,0.2,0.266666666666667,0.333333333333333,
0.4,0.466666666666667,0.533333333333333,0.6,0.666666666666667,0.733333333333333,
0.8,0.866666666666667,0.933333333333333,1.),(0.,1.44),.UNSPECIFIED.);
#62=B_SPLINE_SURFACE_WITH_KNOTS('',3,3,((#22693,#22694,#22695,#22696,#22697,
#22698),(#22699,#22700,#22701,#22702,#22703,#22704),(#22705,#22706,#22707,
#22708,#22709,#22710),(#22711,#22712,#22713,#22714,#22715,#22716),(#22717,
#22718,#22719,#22720,#22721,#22722),(#22723,#22724,#22725,#22726,#22727,
#22728)),.UNSPECIFIED.,.F.,.F.,.F.,(4,1,1,4),(4,1,1,4),(0.,0.285714285714286,
0.571428571428571,1.00003411570466),(-3.41157046611592E-5,0.0348511435350236,
0.0580852392250393,0.0813534506197162),.UNSPECIFIED.);
#63=B_SPLINE_SURFACE_WITH_KNOTS('',3,3,((#22783,#22784,#22785,#22786,#22787,
#22788),(#22789,#22790,#22791,#22792,#22793,#22794),(#22795,#22796,#22797,
#22798,#22799,#22800),(#22801,#22802,#22803,#22804,#22805,#22806),(#22807,
#22808,#22809,#22810,#22811,#22812),(#22813,#22814,#22815,#22816,#22817,
#22818)),.UNSPECIFIED.,.F.,.F.,.F.,(4,1,1,4),(4,1,1,4),(0.,0.285714285714286,
0.571428571428571,1.00010679363949),(-0.000106793639489728,0.0232340956900158,
0.0348511435350236,0.0814261285545448),.UNSPECIFIED.);
#64=B_SPLINE_SURFACE_WITH_KNOTS('',3,3,((#22879,#22880,#22881,#22882,#22883,
#22884),(#22885,#22886,#22887,#22888,#22889,#22890),(#22891,#22892,#22893,
#22894,#22895,#22896),(#22897,#22898,#22899,#22900,#22901,#22902),(#22903,
#22904,#22905,#22906,#22907,#22908)),.UNSPECIFIED.,.F.,.F.,.F.,(4,1,4),
(4,1,1,4),(0.,0.5,1.),(0.,0.0344711845244392,0.0574519742073987,0.0804327638903581),
 .UNSPECIFIED.);
#65=B_SPLINE_SURFACE_WITH_KNOTS('',3,3,((#22930,#22931,#22932,#22933,#22934),
(#22935,#22936,#22937,#22938,#22939),(#22940,#22941,#22942,#22943,#22944),
(#22945,#22946,#22947,#22948,#22949),(#22950,#22951,#22952,#22953,#22954)),
 .UNSPECIFIED.,.F.,.F.,.F.,(4,1,4),(4,1,4),(0.,0.5,1.),(0.,0.0344716480101997,
0.0804338453571326),.UNSPECIFIED.);
#66=B_SPLINE_SURFACE_WITH_KNOTS('',3,3,((#23009,#23010,#23011,#23012,#23013,
#23014,#23015,#23016,#23017,#23018,#23019),(#23020,#23021,#23022,#23023,
#23024,#23025,#23026,#23027,#23028,#23029,#23030),(#23031,#23032,#23033,
#23034,#23035,#23036,#23037,#23038,#23039,#23040,#23041),(#23042,#23043,
#23044,#23045,#23046,#23047,#23048,#23049,#23050,#23051,#23052),(#23053,
#23054,#23055,#23056,#23057,#23058,#23059,#23060,#23061,#23062,#23063)),
 .UNSPECIFIED.,.F.,.F.,.F.,(4,1,4),(4,2,1,1,1,1,1,4),(0.,0.571428571428571,
1.),(-0.00337447822144074,0.,0.252271193732039,0.378406790598058,0.504542387464077,
0.630677984330096,0.756813581196116,0.882949178062135),.UNSPECIFIED.);
#67=B_SPLINE_SURFACE_WITH_KNOTS('',3,1,((#23117,#23118),(#23119,#23120),
(#23121,#23122),(#23123,#23124),(#23125,#23126)),.UNSPECIFIED.,.F.,.F.,
 .F.,(4,1,4),(2,2),(0.,0.5,1.),(0.,0.8715982725842),.UNSPECIFIED.);
#68=B_SPLINE_SURFACE_WITH_KNOTS('',5,1,((#23132,#23133),(#23134,#23135),
(#23136,#23137),(#23138,#23139),(#23140,#23141),(#23142,#23143),(#23144,
#23145),(#23146,#23147),(#23148,#23149),(#23150,#23151),(#23152,#23153),
(#23154,#23155),(#23156,#23157),(#23158,#23159),(#23160,#23161),(#23162,
#23163),(#23164,#23165),(#23166,#23167),(#23168,#23169),(#23170,#23171)),
 .UNSPECIFIED.,.F.,.F.,.F.,(6,1,1,1,1,1,1,1,1,1,1,1,1,1,1,6),(2,2),(0.,
0.0666666666666667,0.133333333333333,0.2,0.266666666666667,0.333333333333333,
0.4,0.466666666666667,0.533333333333333,0.6,0.666666666666667,0.733333333333333,
0.8,0.866666666666667,0.933333333333333,1.),(0.,1.1115982725842),
 .UNSPECIFIED.);
#69=B_SPLINE_SURFACE_WITH_KNOTS('',3,3,((#23214,#23215,#23216,#23217,#23218,
#23219,#23220,#23221,#23222,#23223),(#23224,#23225,#23226,#23227,#23228,
#23229,#23230,#23231,#23232,#23233),(#23234,#23235,#23236,#23237,#23238,
#23239,#23240,#23241,#23242,#23243),(#23244,#23245,#23246,#23247,#23248,
#23249,#23250,#23251,#23252,#23253),(#23254,#23255,#23256,#23257,#23258,
#23259,#23260,#23261,#23262,#23263)),.UNSPECIFIED.,.F.,.F.,.F.,(4,1,4),
(4,2,1,1,1,1,4),(0.,0.571428571428571,1.),(-0.00337447822145283,0.,0.176589835612662,
0.353179671225324,0.529769506837986,0.706359342450648,0.88294917806331),
 .UNSPECIFIED.);
#70=B_SPLINE_SURFACE_WITH_KNOTS('',5,1,((#23446,#23447),(#23448,#23449),
(#23450,#23451),(#23452,#23453),(#23454,#23455),(#23456,#23457),(#23458,
#23459),(#23460,#23461),(#23462,#23463),(#23464,#23465),(#23466,#23467),
(#23468,#23469),(#23470,#23471),(#23472,#23473),(#23474,#23475),(#23476,
#23477),(#23478,#23479),(#23480,#23481),(#23482,#23483),(#23484,#23485),
(#23486,#23487),(#23488,#23489),(#23490,#23491),(#23492,#23493),(#23494,
#23495),(#23496,#23497),(#23498,#23499),(#23500,#23501),(#23502,#23503),
(#23504,#23505),(#23506,#23507),(#23508,#23509),(#23510,#23511)),
 .UNSPECIFIED.,.F.,.F.,.F.,(6,1,1,1,1,1,1,1,1,1,1,1,1,1,1,1,1,1,1,1,1,1,
1,1,1,1,1,1,6),(2,2),(0.45747490134806,0.46,0.48,0.5,0.52,0.54,0.56,0.58,
0.6,0.62,0.64,0.66,0.68,0.7,0.72,0.74,0.76,0.78,0.8,0.82,0.84,0.86,0.88,
0.9,0.92,0.940000000000001,0.960000000000001,0.980000000000001,0.998665134312148),
(0.,0.931560000000001),.UNSPECIFIED.);
#71=B_SPLINE_CURVE_WITH_KNOTS('',3,(#6240,#6241,#6242,#6243,#6244,#6245,
#6246,#6247,#6248,#6249,#6250,#6251,#6252,#6253,#6254,#6255,#6256,#6257,
#6258,#6259,#6260,#6261,#6262,#6263,#6264,#6265,#6266,#6267,#6268,#6269,
#6270,#6271,#6272,#6273,#6274,#6275,#6276,#6277,#6278,#6279,#6280,#6281,
#6282,#6283,#6284,#6285,#6286,#6287,#6288,#6289,#6290,#6291,#6292,#6293,
#6294,#6295,#6296,#6297,#6298,#6299,#6300,#6301,#6302,#6303,#6304,#6305,
#6306,#6307,#6308,#6309,#6310,#6311,#6312,#6313,#6314,#6315,#6316,#6317,
#6318,#6319,#6320,#6321,#6322,#6323,#6324,#6325,#6326,#6327,#6328,#6329,
#6330,#6331,#6332,#6333,#6334,#6335,#6336,#6337,#6338,#6339,#6340,#6341,
#6342,#6343,#6344,#6345,#6346,#6347,#6348,#6349,#6350,#6351,#6352,#6353,
#6354,#6355,#6356,#6357,#6358,#6359,#6360,#6361,#6362,#6363,#6364,#6365,
#6366,#6367,#6368,#6369,#6370,#6371,#6372,#6373,#6374,#6375,#6376,#6377,
#6378,#6379,#6380,#6381,#6382,#6383,#6384,#6385,#6386,#6387,#6388,#6389,
#6390,#6391,#6392,#6393,#6394,#6395,#6396,#6397,#6398,#6399,#6400,#6401,
#6402,#6403,#6404,#6405,#6406,#6407,#6408,#6409,#6410,#6411,#6412,#6413,
#6414,#6415,#6416,#6417,#6418,#6419,#6420,#6421,#6422,#6423,#6424,#6425,
#6426,#6427,#6428,#6429,#6430,#6431,#6432,#6433,#6434,#6435,#6436,#6437,
#6438,#6439),.UNSPECIFIED.,.F.,.F.,(4,2,2,2,2,2,2,2,2,2,2,2,2,2,2,2,2,2,
2,2,2,2,2,2,2,2,2,2,2,2,2,2,2,2,2,2,2,2,2,2,2,2,2,2,2,2,2,2,2,2,2,2,2,2,
2,2,2,2,2,2,2,2,2,2,2,2,2,2,2,2,2,2,2,2,2,2,2,2,2,2,2,2,2,2,2,2,2,2,2,2,
2,2,2,2,2,2,2,2,2,4),(-1.06702706684471,-1.05497244523198,-1.01665474666674,
-0.987326289287207,-0.984035699475469,-0.982343864446482,-0.980993032046556,
-0.979376055011248,-0.976344023459278,-0.957445920983846,-0.930057126831693,
-0.891518695952568,-0.886640257936173,-0.88356711296312,-0.881145191893844,
-0.87843483697744,-0.873892042240304,-0.855680156138417,-0.817294175426114,
-0.788127006009375,-0.784831781483875,-0.78313657234584,-0.781780806435103,
-0.7801543695058,-0.777100119816486,-0.757830693945903,-0.716953969705863,
-0.692298585803861,-0.687665864689332,-0.684663723883678,-0.682243359929601,
-0.679475912798355,-0.67469009538424,-0.65298285297418,-0.608712726286249,
-0.602465225697488,-0.588551357192911,-0.585891842462912,-0.584198945364764,
-0.58285130754978,-0.581247153549654,-0.578238297610785,-0.559520102171982,
-0.531873250013637,-0.493093337940054,-0.488232136921119,-0.485176457771325,
-0.482772740578015,-0.480087609996014,-0.475599336143425,-0.457808496003499,
-0.422846915570689,-0.392139941587043,-0.387236338277925,-0.385224212063848,
-0.383846874449487,-0.382397836822678,-0.380138381095141,-0.373073528948939,
-0.361283740951099,-0.3327770569905,-0.29345629296067,-0.288559857466281,
-0.285473632302045,-0.283040273102544,-0.280315832220917,-0.275745964889562,
-0.257351578317201,-0.218119053870677,-0.190340000473415,-0.187067238723753,
-0.185383087077227,-0.184031961276504,-0.184019005104345,-0.184006411822611,
-0.183994166925342,-0.183982256675038,-0.183970668041925,-0.183959388666292,
-0.183948406811756,-0.18393771133524,-0.183927291637329,-0.183917137641101,
-0.183907239757321,-0.183897588840279,-0.183888176187753,-0.183878993503064,
-0.183870032865609,-0.182192209855574,-0.178902630457108,-0.151793757873708,
-0.107615515621311,-0.0948511658450676,-0.0906278153001035,-0.0879581350487007,
-0.0854704570227276,-0.0821641180987161,-0.0748110605994982,-0.0197428996379006,
-0.00326166647738545),.UNSPECIFIED.);
#72=B_SPLINE_CURVE_WITH_KNOTS('',3,(#6442,#6443,#6444,#6445,#6446,#6447,
#6448,#6449,#6450,#6451,#6452,#6453,#6454,#6455,#6456,#6457,#6458,#6459,
#6460,#6461,#6462,#6463,#6464,#6465,#6466,#6467,#6468,#6469,#6470,#6471,
#6472,#6473,#6474,#6475,#6476,#6477,#6478,#6479,#6480,#6481,#6482,#6483,
#6484,#6485,#6486,#6487,#6488,#6489,#6490,#6491,#6492,#6493,#6494,#6495,
#6496,#6497,#6498,#6499,#6500,#6501,#6502,#6503,#6504,#6505,#6506,#6507,
#6508,#6509,#6510,#6511,#6512,#6513,#6514,#6515,#6516,#6517,#6518,#6519,
#6520,#6521,#6522,#6523,#6524,#6525,#6526,#6527,#6528,#6529,#6530,#6531,
#6532,#6533,#6534,#6535,#6536,#6537,#6538,#6539,#6540,#6541,#6542,#6543,
#6544,#6545,#6546,#6547,#6548,#6549,#6550,#6551,#6552,#6553,#6554,#6555,
#6556,#6557,#6558,#6559,#6560,#6561,#6562,#6563,#6564,#6565),
 .UNSPECIFIED.,.F.,.F.,(4,3,3,3,3,3,3,3,3,3,3,3,3,3,3,3,3,3,3,3,3,3,3,3,
3,3,3,3,3,3,3,3,3,3,3,3,3,3,3,3,3,4),(11.6163931973415,11.7238264230327,
11.8349096544239,11.9422659925758,12.049624554327,12.157014009309,12.2644630561389,
12.3720777239813,12.479788650104,12.5876971425722,12.6124922741621,12.7163982786736,
12.8201309958735,12.9237216952729,13.0272353744651,13.1307090292524,13.2341795975609,
13.337754874388,13.4413864212204,13.5452029841441,13.6085913509826,13.7137335322645,
13.8187189715362,13.923581225803,14.0283775980985,14.1331433556847,14.2379137215731,
14.3427919619306,14.4477304036871,14.5528461722256,14.6046904278032,14.7098521616725,
14.8148608616375,14.9197517921604,15.0245801889838,15.1293812805526,15.2341902545063,
15.3391118366484,15.4440963811367,15.5492620785737,15.6007895046238,15.7079632679489),
 .UNSPECIFIED.);
#73=B_SPLINE_CURVE_WITH_KNOTS('',3,(#6570,#6571,#6572,#6573,#6574,#6575,
#6576,#6577,#6578,#6579,#6580,#6581,#6582,#6583,#6584,#6585,#6586,#6587,
#6588,#6589,#6590,#6591,#6592,#6593,#6594,#6595,#6596,#6597,#6598,#6599,
#6600,#6601,#6602,#6603,#6604,#6605,#6606,#6607,#6608,#6609,#6610,#6611,
#6612,#6613,#6614,#6615,#6616,#6617,#6618,#6619,#6620,#6621,#6622,#6623,
#6624,#6625,#6626,#6627,#6628,#6629,#6630,#6631,#6632,#6633,#6634,#6635,
#6636,#6637,#6638,#6639,#6640,#6641,#6642,#6643,#6644,#6645,#6646,#6647,
#6648,#6649,#6650,#6651,#6652,#6653,#6654,#6655,#6656,#6657,#6658,#6659,
#6660,#6661,#6662,#6663,#6664,#6665,#6666,#6667,#6668,#6669,#6670,#6671,
#6672,#6673,#6674,#6675,#6676,#6677,#6678,#6679,#6680,#6681,#6682,#6683,
#6684,#6685,#6686,#6687,#6688,#6689,#6690,#6691,#6692,#6693,#6694,#6695,
#6696,#6697,#6698,#6699,#6700,#6701,#6702,#6703,#6704,#6705,#6706,#6707,
#6708,#6709,#6710,#6711,#6712,#6713,#6714,#6715,#6716,#6717,#6718,#6719,
#6720,#6721,#6722,#6723,#6724,#6725,#6726,#6727,#6728,#6729,#6730,#6731,
#6732,#6733,#6734,#6735,#6736,#6737,#6738,#6739,#6740,#6741,#6742,#6743,
#6744,#6745,#6746,#6747,#6748,#6749,#6750,#6751,#6752,#6753,#6754,#6755,
#6756,#6757,#6758,#6759,#6760,#6761,#6762,#6763,#6764,#6765,#6766,#6767,
#6768,#6769,#6770,#6771,#6772,#6773,#6774,#6775,#6776,#6777,#6778,#6779,
#6780,#6781,#6782,#6783,#6784,#6785),.UNSPECIFIED.,.F.,.F.,(4,2,2,2,2,2,
2,2,2,2,2,2,2,2,2,2,2,2,2,2,2,2,2,2,2,2,2,2,2,2,2,2,2,2,2,2,2,2,2,2,2,2,
2,2,2,2,2,2,2,2,2,2,2,2,2,2,2,2,2,2,2,2,2,2,2,2,2,2,2,2,2,2,2,2,2,2,2,2,
2,2,2,2,2,2,2,2,2,2,2,2,2,2,2,2,2,2,2,2,2,2,2,2,2,2,2,2,2,4),(-2.32340959930946,
-2.28671636369838,-2.28248129744248,-2.27965891672853,-2.27693862878967,
-2.27452011257343,-2.27146787835447,-2.26665554316793,-2.23659007898717,
-2.21249762971968,-2.18721978508259,-2.18035006287128,-2.1786597848142,
-2.17707240687928,-2.17571851532218,-2.1739871568661,-2.17119871447672,
-2.15466375160865,-2.13944937897683,-2.10277442830581,-2.08511469724236,
-2.08063747906312,-2.07789290905577,-2.07547780793399,-2.07246298493117,
-2.06777407196391,-2.04162762789115,-1.99753434182706,-1.98238247027529,
-1.9795052533592,-1.97792113172633,-1.9765666369363,-1.97483016455707,-1.9720252427692,
-1.95510039498244,-1.9063563954152,-1.88613155885719,-1.88144786392857,
-1.878707466285,-1.87629158113081,-1.87326989701188,-1.86855889754755,-1.84168264898425,
-1.80246384200122,-1.78348742316995,-1.78045226843756,-1.77883440396489,
-1.77748286913533,-1.77579018853629,-1.77249907620905,-1.74350934759795,
-1.70496738168487,-1.68671566353333,-1.68217177739531,-1.67946232182981,
-1.6770421873822,-1.67397266025881,-1.6691026108338,-1.62996536702173,-1.60194124700158,
-1.58425036261844,-1.5812625181024,-1.5796548511277,-1.57830278235529,-1.57659803562786,
-1.57389780788538,-1.55917593961205,-1.50834421545852,-1.48781339863567,
-1.48310987743816,-1.48036526274816,-1.47795011067682,-1.47493520880341,
-1.47024613712677,-1.44415838630842,-1.40425113971119,-1.3851521755854,
-1.38211255345633,-1.38049361187249,-1.37914138825622,-1.37744816709172,
-1.37415834136411,-1.34688282072237,-1.31193012843637,-1.28899672785052,
-1.28414858328718,-1.28137166068175,-1.27895862638588,-1.27598574083246,
-1.27143654482001,-1.24862377933376,-1.20573232481638,-1.18607028815224,
-1.1830119430291,-1.18138904228055,-1.180038348652,-1.17835296608331,-1.17571358020806,
-1.16210930303577,-1.12849464709001,-1.12385634376739,-1.09076801866163,
-1.08589923643028,-1.08283140791067,-1.0804132315342,-1.07770664095782,
-1.07316925509502,-1.06702706684471),.UNSPECIFIED.);
#74=B_SPLINE_CURVE_WITH_KNOTS('',3,(#6786,#6787,#6788,#6789,#6790,#6791,
#6792,#6793,#6794,#6795),.UNSPECIFIED.,.F.,.F.,(4,1,1,1,1,1,1,4),(15.7079719615557,
16.5968885814444,17.592987658265,18.5890867350856,19.5851858119062,20.5812848887268,
21.5773839655474,21.9911426286453),.UNSPECIFIED.);
#75=B_SPLINE_CURVE_WITH_KNOTS('',3,(#6800,#6801,#6802,#6803,#6804,#6805,
#6806,#6807,#6808,#6809,#6810),.UNSPECIFIED.,.F.,.F.,(4,1,1,1,1,1,1,1,4),
(21.9911513165397,22.2535448026509,23.2496438794715,24.2457429562921,25.2418420331127,
26.2379411099333,27.2340401867539,28.2301392635745,28.2743338823081),
 .UNSPECIFIED.);
#76=B_SPLINE_CURVE_WITH_KNOTS('',3,(#6811,#6812,#6813,#6814,#6815,#6816,
#6817,#6818,#6819,#6820,#6821,#6822,#6823,#6824,#6825,#6826,#6827,#6828,
#6829,#6830,#6831,#6832,#6833,#6834,#6835,#6836,#6837,#6838,#6839,#6840,
#6841,#6842,#6843,#6844,#6845,#6846,#6847,#6848,#6849,#6850,#6851,#6852,
#6853,#6854,#6855,#6856,#6857,#6858,#6859,#6860,#6861,#6862,#6863,#6864,
#6865,#6866,#6867,#6868,#6869,#6870,#6871,#6872,#6873,#6874,#6875,#6876,
#6877,#6878,#6879,#6880,#6881,#6882,#6883,#6884,#6885,#6886,#6887,#6888,
#6889,#6890,#6891,#6892,#6893,#6894,#6895,#6896,#6897,#6898,#6899,#6900,
#6901,#6902,#6903,#6904,#6905,#6906,#6907,#6908,#6909,#6910,#6911,#6912,
#6913,#6914,#6915,#6916,#6917,#6918,#6919,#6920,#6921,#6922,#6923,#6924,
#6925,#6926,#6927,#6928,#6929,#6930,#6931,#6932,#6933,#6934,#6935,#6936,
#6937,#6938,#6939,#6940,#6941,#6942,#6943,#6944,#6945,#6946,#6947,#6948,
#6949,#6950,#6951,#6952,#6953,#6954,#6955,#6956,#6957,#6958,#6959,#6960,
#6961,#6962,#6963,#6964,#6965,#6966,#6967,#6968,#6969,#6970,#6971,#6972,
#6973,#6974,#6975,#6976,#6977,#6978,#6979,#6980,#6981,#6982,#6983,#6984,
#6985,#6986,#6987,#6988,#6989,#6990,#6991,#6992,#6993,#6994,#6995,#6996,
#6997,#6998,#6999,#7000,#7001,#7002,#7003,#7004,#7005,#7006,#7007,#7008,
#7009,#7010,#7011,#7012,#7013,#7014,#7015,#7016,#7017,#7018,#7019,#7020,
#7021,#7022,#7023,#7024),.UNSPECIFIED.,.F.,.F.,(4,2,2,2,2,2,2,2,2,2,2,2,
2,2,2,2,2,2,2,2,2,2,2,2,2,2,2,2,2,2,2,2,2,2,2,2,2,2,2,2,2,2,2,2,2,2,2,2,
2,2,2,2,2,2,2,2,2,2,2,2,2,2,2,2,2,2,2,2,2,2,2,2,2,2,2,2,2,2,2,2,2,2,2,2,
2,2,2,2,2,2,2,2,2,2,2,2,2,2,2,2,2,2,2,2,2,2,4),(-2.51309494483192,-2.50320433340691,
-2.50019787928662,-2.49785177109079,-2.49550498564395,-2.49282979160281,
-2.48843898141752,-2.47384060084744,-2.42194777797328,-2.40189155767509,
-2.39882211610243,-2.39719746300626,-2.39584663860536,-2.39416288679831,
-2.39091279089183,-2.36757483483152,-2.33376985310361,-2.31537020214508,
-2.30764205148646,-2.30341567186313,-2.30059702444992,-2.29792694834691,
-2.29552962168192,-2.29250872221,-2.28779901889248,-2.26101007604918,-2.22174029788307,
-2.20275780425738,-2.19972287803772,-2.19810522711465,-2.19675385483173,
-2.19506135474195,-2.19177069455665,-2.16461620159165,-2.1295625510239,
-2.10658487398944,-2.10173642498569,-2.09896061732351,-2.09654932345174,
-2.09357958747997,-2.08903712860248,-2.06633021779805,-2.02336650079388,
-2.00369168254696,-2.00063383957115,-1.99901142479705,-1.99766033119149,
-1.99597354539965,-1.99270954662011,-1.96844581156467,-1.94048542244649,
-1.91108748436525,-1.90401549717365,-1.90079413463281,-1.89835452747676,
-1.89604333300452,-1.89214825145016,-1.88155714034897,-1.82104861712037,
-1.80432941469198,-1.80138075665389,-1.7997813507419,-1.79842851345984,
-1.79671293895133,-1.79397714704231,-1.77852371766808,-1.76162225748251,
-1.73074318883517,-1.7082451939056,-1.70342251211113,-1.70065184694556,
-1.69823939328664,-1.69526100457241,-1.69069169413982,-1.66738212550672,
-1.62964936886666,-1.60768027718677,-1.60312219347139,-1.60121615038319,
-1.5998395703432,-1.5985329369825,-1.59626057400744,-1.58969794624879,-1.5309160670397,
-1.50897570716499,-1.50418559679285,-1.50142222147116,-1.49900938265331,
-1.49602182559183,-1.49142197040518,-1.46739752772076,-1.42560857916681,
-1.40616692047357,-1.4031163078847,-1.40149526522063,-1.40014388511311,
-1.39845494691612,-1.39518165099361,-1.36532076346427,-1.32744775589378,
-1.30935574142146,-1.30482375826102,-1.30211677582176,-1.29969595313211,
-1.29662160012855,-1.29173594442689,-1.25689120554917),.UNSPECIFIED.);
#77=B_SPLINE_CURVE_WITH_KNOTS('',3,(#7029,#7030,#7031,#7032,#7033,#7034,
#7035,#7036,#7037,#7038,#7039,#7040,#7041,#7042,#7043,#7044,#7045,#7046,
#7047,#7048,#7049,#7050,#7051,#7052,#7053,#7054,#7055,#7056,#7057,#7058,
#7059,#7060,#7061,#7062,#7063,#7064,#7065,#7066,#7067,#7068,#7069,#7070,
#7071,#7072,#7073,#7074,#7075,#7076,#7077,#7078,#7079,#7080,#7081,#7082,
#7083,#7084,#7085,#7086,#7087,#7088,#7089,#7090,#7091,#7092,#7093,#7094,
#7095,#7096,#7097,#7098,#7099,#7100,#7101,#7102,#7103,#7104,#7105,#7106,
#7107,#7108,#7109,#7110,#7111,#7112,#7113,#7114,#7115,#7116,#7117,#7118,
#7119,#7120,#7121,#7122,#7123,#7124,#7125,#7126,#7127,#7128,#7129,#7130,
#7131,#7132,#7133,#7134,#7135,#7136,#7137,#7138,#7139,#7140,#7141,#7142,
#7143,#7144,#7145,#7146,#7147,#7148,#7149,#7150,#7151,#7152,#7153,#7154,
#7155,#7156,#7157,#7158,#7159,#7160,#7161,#7162,#7163,#7164,#7165,#7166,
#7167,#7168,#7169,#7170,#7171,#7172,#7173,#7174,#7175,#7176,#7177,#7178,
#7179,#7180,#7181,#7182,#7183,#7184,#7185,#7186,#7187,#7188,#7189,#7190,
#7191,#7192,#7193,#7194,#7195,#7196,#7197,#7198,#7199,#7200,#7201,#7202,
#7203,#7204,#7205,#7206,#7207,#7208,#7209,#7210,#7211,#7212,#7213,#7214,
#7215),.UNSPECIFIED.,.F.,.F.,(4,3,3,3,3,3,3,3,3,3,3,3,3,3,3,3,3,3,3,3,3,
3,3,3,3,3,3,3,3,3,3,3,3,3,3,3,3,3,3,3,3,3,3,3,3,3,3,3,3,3,3,3,3,3,3,3,3,
3,3,3,3,3,4),(28.2743342502764,28.3785778767343,28.4845354346919,28.5885092029038,
28.6924238812719,28.7963159943847,28.9037965808873,29.0078182645905,29.1170283024928,
29.2262383403951,29.3312185781844,29.4360418397988,29.5407424118362,29.6453775156852,
29.7499826790951,29.8545933861702,29.9593145177744,30.0640970811506,30.1690605520178,
30.2223374172156,30.3273176545636,30.432140915713,30.536841487253,30.6414765905846,
30.7460817534581,30.8506924599781,30.9554135910029,31.060196153785,31.1651596240413,
31.2184364940362,31.3234167330088,31.4282399958122,31.5329405690411,31.6375756740824,
31.7421808386837,31.8467915469473,31.9515126797276,32.0562952442743,32.1612587162913,
32.2145355708568,32.3195158090238,32.4243390710114,32.5290396434136,32.6336747476218,
32.7382799113848,32.8428906188066,32.9476117507447,33.0523943144481,33.1573577856286,
33.2106346476774,33.3156148858565,33.4204381478543,33.5251387202629,33.6297738244755,
33.7343789882406,33.8389896956618,33.9437108275967,34.048493391295,34.1534568624678,
34.206733724498,34.3277897537902,34.4478095797928,34.5575191891054),
 .UNSPECIFIED.);
#78=B_SPLINE_CURVE_WITH_KNOTS('',3,(#7216,#7217,#7218,#7219,#7220,#7221,
#7222,#7223,#7224,#7225,#7226,#7227,#7228,#7229,#7230,#7231,#7232,#7233,
#7234,#7235,#7236,#7237,#7238,#7239,#7240,#7241,#7242,#7243,#7244,#7245,
#7246,#7247,#7248,#7249,#7250,#7251,#7252,#7253,#7254,#7255,#7256,#7257,
#7258,#7259,#7260,#7261,#7262,#7263,#7264,#7265,#7266,#7267,#7268,#7269,
#7270,#7271,#7272,#7273,#7274,#7275,#7276,#7277,#7278,#7279,#7280,#7281,
#7282,#7283,#7284,#7285,#7286,#7287,#7288,#7289,#7290,#7291,#7292,#7293,
#7294,#7295,#7296,#7297,#7298,#7299,#7300,#7301,#7302,#7303,#7304,#7305,
#7306,#7307,#7308,#7309,#7310,#7311,#7312,#7313,#7314,#7315,#7316,#7317,
#7318,#7319,#7320,#7321,#7322,#7323,#7324,#7325,#7326,#7327,#7328,#7329,
#7330,#7331,#7332,#7333,#7334,#7335,#7336,#7337,#7338,#7339,#7340,#7341,
#7342,#7343,#7344,#7345,#7346,#7347,#7348,#7349,#7350,#7351,#7352,#7353,
#7354,#7355,#7356,#7357,#7358,#7359,#7360,#7361,#7362,#7363,#7364,#7365,
#7366,#7367,#7368,#7369,#7370,#7371,#7372,#7373,#7374,#7375,#7376,#7377,
#7378,#7379,#7380,#7381,#7382,#7383,#7384,#7385,#7386,#7387,#7388,#7389,
#7390,#7391,#7392,#7393,#7394,#7395,#7396,#7397,#7398,#7399,#7400,#7401,
#7402,#7403,#7404,#7405,#7406,#7407,#7408,#7409,#7410,#7411,#7412,#7413,
#7414,#7415,#7416,#7417,#7418,#7419,#7420,#7421,#7422,#7423,#7424,#7425,
#7426,#7427,#7428,#7429,#7430,#7431,#7432,#7433,#7434,#7435,#7436,#7437),
 .UNSPECIFIED.,.F.,.F.,(4,2,2,2,2,2,2,2,2,2,2,2,2,2,2,2,2,2,2,2,2,2,2,2,
2,2,2,2,2,2,2,2,2,2,2,2,2,2,2,2,2,2,2,2,2,2,2,2,2,2,2,2,2,2,2,2,2,2,2,2,
2,2,2,2,2,2,2,2,2,2,2,2,2,2,2,2,2,2,2,2,2,2,2,2,2,2,2,2,2,2,2,2,2,2,2,2,
2,2,2,2,2,2,2,2,2,2,2,2,2,2,4),(-1.25689120554917,-1.25671098397983,-1.25066044802923,
-1.20948522782805,-1.20491064445208,-1.20313714588804,-1.20185997527627,
-1.2004620937551,-1.1984396770067,-1.19314793368247,-1.18522029099217,-1.15865145486666,
-1.11497401188691,-1.10749967291772,-1.1045350791722,-1.10206941300667,
-1.09953631713358,-1.09580841404871,-1.08553719558386,-1.06994272249528,
-1.03560901274684,-1.00833242892861,-1.00504044381963,-1.00334745473176,
-1.00199584896178,-1.00037812612067,-0.997343437119441,-0.97837365130018,
-0.939151505365429,-0.912314034499537,-0.90760486837056,-0.904583841567298,
-0.902168168109199,-0.899427675624065,-0.894742998744615,-0.874501760959482,
-0.82567343419625,-0.808798879247274,-0.805995983750893,-0.804260196634177,
-0.802905814611509,-0.801321299904463,-0.798442302725255,-0.783252762889681,
-0.753093879630736,-0.713432025708798,-0.708566812426657,-0.705498458347683,
-0.703078089345408,-0.700367155226849,-0.69581786263213,-0.677501968708486,
-0.638690514808245,-0.610001750157104,-0.60671002913905,-0.605017031403042,
-0.603665339561002,-0.602047419014631,-0.599012110817107,-0.580029059989649,
-0.540736854294525,-0.513972503916871,-0.509265608884649,-0.506245163496234,
-0.503829392631909,-0.501088185318222,-0.49640077874294,-0.476121567928966,
-0.427048959552658,-0.41043452728958,-0.407642254046349,-0.405909586891387,
-0.404555367457733,-0.402968399167106,-0.400078334183035,-0.384663324279011,
-0.338508660130861,-0.314557277020408,-0.309960253739445,-0.30697328265707,
-0.304560112473025,-0.301795474673092,-0.297000917839606,-0.2749969507767,
-0.245530882454,-0.214093558884376,-0.209207553265977,-0.207183881735866,
-0.20583567815469,-0.204425498993356,-0.202279294029855,-0.199752654919245,
-0.194972367863382,-0.183059314699426,-0.155048145856931,-0.115924458706309,
-0.111054912861928,-0.107985187605656,-0.105564587246349,-0.102854282099866,
-0.0983081779359894,-0.0800363803910931,-0.0266261906942104,-0.0178723290072204,
-0.0107036920865427,-0.0083518670699158,-0.00688327807733598,-0.00559729557625789,
-0.00422686291420059,-0.00239437268791312,-0.000585284694235494),
 .UNSPECIFIED.);
#79=B_SPLINE_CURVE_WITH_KNOTS('',3,(#7442,#7443,#7444,#7445,#7446,#7447,
#7448,#7449,#7450,#7451,#7452,#7453,#7454,#7455,#7456,#7457,#7458,#7459,
#7460,#7461,#7462,#7463,#7464,#7465,#7466,#7467,#7468,#7469,#7470,#7471,
#7472,#7473,#7474,#7475,#7476,#7477,#7478,#7479,#7480,#7481,#7482,#7483,
#7484,#7485,#7486,#7487,#7488,#7489,#7490,#7491,#7492,#7493,#7494,#7495,
#7496,#7497,#7498,#7499,#7500,#7501,#7502,#7503,#7504,#7505,#7506,#7507,
#7508,#7509,#7510,#7511,#7512,#7513,#7514,#7515,#7516,#7517,#7518,#7519,
#7520,#7521,#7522,#7523,#7524,#7525,#7526,#7527,#7528,#7529,#7530,#7531,
#7532,#7533,#7534,#7535,#7536,#7537,#7538,#7539,#7540,#7541,#7542,#7543,
#7544,#7545,#7546,#7547,#7548,#7549,#7550,#7551,#7552,#7553,#7554,#7555,
#7556,#7557,#7558,#7559,#7560,#7561,#7562,#7563,#7564,#7565,#7566,#7567,
#7568,#7569,#7570,#7571,#7572,#7573,#7574,#7575,#7576,#7577,#7578,#7579,
#7580,#7581,#7582,#7583,#7584,#7585,#7586,#7587,#7588,#7589,#7590,#7591,
#7592,#7593,#7594,#7595,#7596,#7597,#7598,#7599,#7600,#7601,#7602,#7603,
#7604,#7605,#7606,#7607,#7608,#7609,#7610,#7611,#7612,#7613,#7614,#7615,
#7616,#7617,#7618,#7619,#7620,#7621,#7622,#7623,#7624,#7625,#7626,#7627,
#7628,#7629,#7630,#7631,#7632,#7633,#7634,#7635,#7636,#7637,#7638,#7639,
#7640,#7641,#7642,#7643,#7644,#7645,#7646,#7647,#7648,#7649,#7650,#7651,
#7652,#7653,#7654,#7655,#7656,#7657,#7658,#7659,#7660,#7661,#7662,#7663,
#7664,#7665,#7666,#7667,#7668,#7669,#7670,#7671,#7672,#7673,#7674,#7675,
#7676,#7677,#7678,#7679,#7680,#7681,#7682,#7683,#7684,#7685,#7686,#7687,
#7688,#7689,#7690,#7691),.UNSPECIFIED.,.F.,.F.,(4,2,2,2,2,2,2,2,2,2,2,2,
2,2,2,2,2,2,2,2,2,2,2,2,2,2,2,2,2,2,2,2,2,2,2,2,2,2,2,2,2,2,2,2,2,2,2,2,
2,2,2,2,2,2,2,2,2,2,2,2,2,2,2,2,2,2,2,2,2,2,2,2,2,2,2,2,2,2,2,2,2,2,2,2,
2,2,2,2,2,2,2,2,2,2,2,2,2,2,2,2,2,2,2,2,2,2,2,2,2,2,2,2,2,2,2,2,2,2,2,2,
2,2,2,2,4),(-1.25717479450333,-1.23431056484724,-1.22975477569507,-1.22678054944049,
-1.22436841538287,-1.22159474466381,-1.21675809941997,-1.19401259331354,
-1.16021307921353,-1.13148317515821,-1.12819157215222,-1.12649863706517,
-1.12514699650765,-1.12352913894593,-1.12049395237826,-1.10151179584398,
-1.06222206626641,-1.03545762467368,-1.03075087072106,-1.0277305290092,
-1.02531484952289,-1.02257375499927,-1.0178865640463,-0.997608684184581,
-0.948541670039921,-0.931923802857341,-0.929131466211711,-0.927398814363777,
-0.926044642690412,-0.924457771968533,-0.921567989602578,-0.906157170600152,
-0.860033563716474,-0.836052505565535,-0.831454332862117,-0.828467069765009,
-0.82605396160448,-0.8232897216895,-0.818496693530489,-0.796516560014088,
-0.737326863349453,-0.731073448412038,-0.728843814010007,-0.727545450200212,
-0.726163481855453,-0.724227296142887,-0.719488270966462,-0.695702774494737,
-0.679155461596489,-0.640743746252026,-0.633293557539204,-0.630251683469711,
-0.627991266980409,-0.625516506249222,-0.622089123662714,-0.613827449226716,
-0.602185789962517,-0.56790593347784,-0.53632536965187,-0.531426598993216,
-0.529407892772127,-0.528024368104393,-0.526574326407731,-0.524306823481104,
-0.517162211647707,-0.505172314606505,-0.477240323994236,-0.438142731879105,
-0.433271125601501,-0.430200515287726,-0.427779475435338,-0.425068948024601,
-0.420523118782819,-0.402261897213763,-0.363691817302333,-0.334681513384031,
-0.33138893403705,-0.3296955492682,-0.328343577946666,-0.326725358185739,
-0.323689582622493,-0.304707168327515,-0.264848431712814,-0.238617051112021,
-0.233916717716315,-0.230897945074816,-0.22848188025595,-0.228432726354342,
-0.228387434695292,-0.228345693394845,-0.228307216353647,-0.228271741174546,
-0.228239027215165,-0.228208853768559,-0.228181018386339,-0.228155335325058,
-0.228131634121797,-0.228109758296482,-0.22808956415974,-0.22807091971706,
-0.228042251455893,-0.228014073274487,-0.227986373900511,-0.225103190176611,
-0.219678869078645,-0.212818374838106,-0.197378730231605,-0.161999562734522,
-0.135487173969977,-0.132197080243353,-0.130504231846451,-0.129152288852188,
-0.127533625846504,-0.124495736849805,-0.10545142468155,-0.0645853483016401,
-0.0484315983646425,-0.0371236971762454,-0.0331271488265467,-0.0305367455272384,
-0.0282310577993952,-0.0258381911911154,-0.0226944350006336,-0.0147032960217883,
-0.000585062358029298),.UNSPECIFIED.);
#80=B_SPLINE_CURVE_WITH_KNOTS('',3,(#7692,#7693,#7694,#7695,#7696,#7697,
#7698,#7699,#7700,#7701,#7702,#7703,#7704,#7705,#7706,#7707,#7708,#7709,
#7710,#7711,#7712,#7713,#7714,#7715,#7716,#7717,#7718,#7719,#7720,#7721,
#7722,#7723,#7724,#7725,#7726,#7727,#7728,#7729,#7730,#7731,#7732,#7733,
#7734,#7735,#7736,#7737,#7738,#7739,#7740,#7741,#7742,#7743,#7744,#7745,
#7746,#7747,#7748,#7749,#7750,#7751,#7752,#7753,#7754,#7755,#7756,#7757,
#7758,#7759,#7760,#7761,#7762,#7763,#7764,#7765,#7766,#7767,#7768,#7769,
#7770,#7771,#7772,#7773,#7774,#7775,#7776,#7777,#7778,#7779,#7780,#7781,
#7782,#7783,#7784,#7785,#7786,#7787,#7788,#7789,#7790,#7791,#7792,#7793,
#7794,#7795,#7796,#7797,#7798,#7799,#7800,#7801,#7802,#7803,#7804,#7805,
#7806,#7807,#7808,#7809,#7810,#7811,#7812,#7813,#7814,#7815,#7816,#7817,
#7818,#7819,#7820,#7821,#7822,#7823,#7824,#7825,#7826,#7827,#7828,#7829,
#7830,#7831,#7832,#7833,#7834,#7835,#7836,#7837,#7838,#7839,#7840,#7841,
#7842,#7843,#7844,#7845,#7846,#7847,#7848,#7849,#7850,#7851,#7852,#7853,
#7854,#7855,#7856,#7857,#7858,#7859,#7860,#7861,#7862,#7863,#7864,#7865,
#7866,#7867,#7868,#7869,#7870,#7871,#7872,#7873,#7874,#7875,#7876,#7877,
#7878,#7879,#7880,#7881,#7882,#7883,#7884,#7885,#7886,#7887,#7888,#7889,
#7890,#7891,#7892,#7893,#7894,#7895,#7896,#7897,#7898,#7899,#7900,#7901,
#7902,#7903,#7904,#7905,#7906,#7907),.UNSPECIFIED.,.F.,.F.,(4,2,2,2,2,2,
2,2,2,2,2,2,2,2,2,2,2,2,2,2,2,2,2,2,2,2,2,2,2,2,2,2,2,2,2,2,2,2,2,2,2,2,
2,2,2,2,2,2,2,2,2,2,2,2,2,2,2,2,2,2,2,2,2,2,2,2,2,2,2,2,2,2,2,2,2,2,2,2,
2,2,2,2,2,2,2,2,2,2,2,2,2,2,2,2,2,2,2,2,2,2,2,2,2,2,2,2,2,4),(-2.5138436186102,
-2.50952290300276,-2.46075586215554,-2.43239072266,-2.4254435661833,-2.42224457440169,
-2.41980775736968,-2.41716430191943,-2.41292249225143,-2.39966904025624,
-2.34835617248966,-2.33322200277272,-2.32761287541776,-2.32478544366912,
-2.32302213034665,-2.32140586879113,-2.32139905251692,-2.32139207186411,
-2.32138492080939,-2.3213775930576,-2.32137008196787,-2.32005598096186,
-2.31839773972454,-2.31533221902634,-2.29803560248755,-2.24962156045713,
-2.22944579027585,-2.2247651855837,-2.22202540545508,-2.21960934763307,
-2.21658650274317,-2.21187186281261,-2.18489498256755,-2.1457610336291,
-2.12679838350396,-2.1237635189943,-2.12214564261047,-2.12079387038351,
-2.11910063177515,-2.11580804131143,-2.08867142589064,-2.05418327682725,
-2.03861854056218,-2.02836017125334,-2.02463372982322,-2.02210069156468,
-2.01963436290226,-2.01666809299148,-2.00918480243566,-1.96564164877097,
-1.93893477140375,-1.93098322869654,-1.92567984285703,-1.92365549682557,
-1.92225709483955,-1.92098008269896,-1.91920765554693,-1.91464082076545,
-1.87337137287138,-1.83300611226229,-1.82721059192544,-1.82423455625505,
-1.82182209420408,-1.81904930550816,-1.81434173957802,-1.79574953865952,
-1.74420812989008,-1.72819568158449,-1.7252775078336,-1.72368441638485,
-1.7223306921472,-1.72060600608063,-1.7178405800224,-1.70185817745435,-1.65222398183631,
-1.63186290377256,-1.62716987086098,-1.62442725197271,-1.62201136820524,
-1.61899227396319,-1.6142903369892,-1.58769008859952,-1.54399973624458,
-1.52890042064648,-1.52602543291397,-1.52444163189966,-1.52308691929542,
-1.52134950800907,-1.51854169815103,-1.50155026530522,-1.45284936562663,
-1.43262818781638,-1.42794430751206,-1.42520367049628,-1.42278749814761,
-1.41976535707357,-1.4150534604555,-1.38816525552912,-1.34894644173208,
-1.32996774733639,-1.32693213429148,-1.32531401923095,-1.32396214122059,
-1.32226888777097,-1.31897660759628,-1.29158969906332,-1.25739797810809,
-1.25725532263633),.UNSPECIFIED.);
#81=B_SPLINE_CURVE_WITH_KNOTS('',3,(#7912,#7913,#7914,#7915,#7916,#7917,
#7918,#7919,#7920,#7921,#7922,#7923,#7924,#7925,#7926,#7927,#7928,#7929,
#7930,#7931,#7932,#7933,#7934,#7935,#7936,#7937,#7938,#7939,#7940,#7941,
#7942,#7943,#7944,#7945,#7946,#7947,#7948,#7949,#7950,#7951,#7952,#7953,
#7954,#7955,#7956,#7957,#7958,#7959,#7960,#7961,#7962,#7963,#7964,#7965,
#7966,#7967,#7968,#7969,#7970,#7971,#7972,#7973,#7974,#7975,#7976,#7977,
#7978,#7979,#7980,#7981,#7982,#7983,#7984,#7985,#7986,#7987,#7988,#7989,
#7990,#7991,#7992,#7993,#7994,#7995,#7996,#7997,#7998,#7999,#8000,#8001,
#8002,#8003,#8004,#8005,#8006,#8007,#8008,#8009,#8010,#8011,#8012,#8013,
#8014,#8015,#8016,#8017,#8018,#8019,#8020,#8021,#8022,#8023,#8024,#8025,
#8026,#8027,#8028,#8029,#8030,#8031,#8032,#8033,#8034,#8035,#8036,#8037,
#8038,#8039,#8040,#8041,#8042,#8043,#8044,#8045,#8046,#8047,#8048,#8049,
#8050,#8051,#8052,#8053,#8054,#8055,#8056,#8057,#8058,#8059,#8060,#8061,
#8062,#8063,#8064,#8065,#8066,#8067,#8068,#8069,#8070,#8071,#8072,#8073,
#8074,#8075,#8076,#8077,#8078,#8079,#8080,#8081,#8082,#8083,#8084,#8085,
#8086,#8087,#8088,#8089,#8090,#8091,#8092,#8093,#8094,#8095,#8096,#8097,
#8098,#8099,#8100,#8101,#8102,#8103,#8104,#8105,#8106,#8107,#8108,#8109,
#8110,#8111,#8112,#8113,#8114,#8115,#8116,#8117,#8118,#8119,#8120,#8121,
#8122,#8123,#8124,#8125,#8126,#8127,#8128,#8129,#8130,#8131,#8132,#8133,
#8134,#8135,#8136,#8137,#8138,#8139,#8140,#8141,#8142,#8143,#8144,#8145,
#8146,#8147,#8148,#8149),.UNSPECIFIED.,.F.,.F.,(4,2,2,2,2,2,2,2,2,2,2,2,
2,2,2,2,2,2,2,2,2,2,2,2,2,2,2,2,2,2,2,2,2,2,2,2,2,2,2,2,2,2,2,2,2,2,2,2,
2,2,2,2,2,2,2,2,2,2,2,2,2,2,2,2,2,2,2,2,2,2,2,2,2,2,2,2,2,2,2,2,2,2,2,2,
2,2,2,2,2,2,2,2,2,2,2,2,2,2,2,2,2,2,2,2,2,2,2,2,2,2,2,2,2,2,2,2,2,2,4),
(-2.51335624080557,-2.506478946999,-2.48359052154761,-2.46127006800987,
-2.43234350190882,-2.42532888506851,-2.42211819499271,-2.41968037468292,
-2.41704350343578,-2.41282902361346,-2.39979778345691,-2.34825978506285,
-2.33311207445996,-2.32750032497869,-2.32467225188235,-2.32290888658861,
-2.32129271795892,-2.32128423243568,-2.32127743880788,-2.32127047540276,
-2.3212633359424,-2.32125601385886,-2.32124850222344,-2.32124079375284,
-2.32123288076894,-2.32122475516387,-2.32121640839591,-2.32120783146814,
-2.32119901485306,-2.32118994846965,-2.32118062165022,-2.3211710230933,
-2.3198578342817,-2.31815829415088,-2.31490885758603,-2.28581119154219,
-2.24735536733383,-2.22912577229372,-2.22458385700287,-2.22187497383776,
-2.21945496987617,-2.21638508520208,-2.21151340680533,-2.17243313090189,
-2.14453309376102,-2.1325095296761,-2.12535245094867,-2.12308413885026,
-2.12163435644588,-2.12025172756361,-2.11823533165146,-2.11334718851118,
-2.08325711360966,-2.05836301572525,-2.03336328455782,-2.02684808899443,
-2.02373054819745,-2.02130502030909,-2.01862274469822,-2.01420229989519,
-1.99932106227157,-1.95523663019295,-1.93038506804559,-1.92554583230165,
-1.923593857263,-1.92220945667648,-1.92073500747957,-1.9183553192337,-1.9109674070567,
-1.87029614475397,-1.84470225126122,-1.83026840771902,-1.82605510739743,
-1.823418252238,-1.82097995530959,-1.81782230715817,-1.81116430095981,-1.7588676691359,
-1.72935922744648,-1.72579391406116,-1.72406810981814,-1.72271465288763,
-1.72112320264002,-1.71829083394295,-1.70568188525691,-1.66138249721186,
-1.63528057508497,-1.62862012767713,-1.62547485602977,-1.62304568967479,
-1.62037742570763,-1.61602133933637,-1.60176155277982,-1.54555753571123,
-1.5291376692443,-1.52620177945079,-1.52460506070798,-1.52325193894913,
-1.52153272906904,-1.51878495980244,-1.50309684492989,-1.45319251212588,
-1.4327944978104,-1.42809965828995,-1.42535695329302,-1.42294157832999,
-1.41992389058856,-1.41522563737345,-1.38871405515121,-1.34916894689295,
-1.33013466670157,-1.32709759769582,-1.32547935957664,-1.32412775977318,
-1.32243533346523,-1.31914604045768,-1.29256993657596,-1.25731654093721,
-1.25717479450333),.UNSPECIFIED.);
#82=B_SPLINE_CURVE_WITH_KNOTS('',3,(#8150,#8151,#8152,#8153,#8154,#8155,
#8156,#8157,#8158,#8159,#8160,#8161,#8162,#8163,#8164,#8165,#8166,#8167,
#8168,#8169,#8170,#8171,#8172,#8173,#8174,#8175,#8176,#8177,#8178,#8179,
#8180,#8181,#8182,#8183,#8184,#8185,#8186,#8187,#8188,#8189,#8190,#8191,
#8192,#8193,#8194,#8195,#8196,#8197,#8198,#8199,#8200,#8201,#8202,#8203,
#8204,#8205,#8206,#8207,#8208,#8209,#8210,#8211,#8212,#8213,#8214,#8215,
#8216,#8217,#8218,#8219,#8220,#8221,#8222,#8223,#8224,#8225,#8226,#8227,
#8228,#8229,#8230,#8231,#8232,#8233,#8234,#8235,#8236,#8237,#8238,#8239,
#8240,#8241,#8242,#8243,#8244,#8245,#8246,#8247,#8248,#8249,#8250,#8251,
#8252,#8253,#8254,#8255,#8256,#8257,#8258,#8259,#8260,#8261,#8262,#8263,
#8264,#8265,#8266,#8267,#8268,#8269,#8270,#8271,#8272,#8273,#8274,#8275,
#8276,#8277,#8278,#8279,#8280,#8281,#8282,#8283,#8284,#8285,#8286,#8287,
#8288,#8289,#8290,#8291,#8292,#8293,#8294,#8295,#8296,#8297,#8298,#8299,
#8300,#8301,#8302,#8303,#8304,#8305,#8306,#8307,#8308,#8309,#8310,#8311,
#8312,#8313,#8314,#8315,#8316,#8317,#8318,#8319,#8320,#8321,#8322,#8323,
#8324,#8325,#8326,#8327,#8328,#8329,#8330,#8331,#8332,#8333,#8334,#8335,
#8336,#8337,#8338,#8339,#8340,#8341,#8342,#8343,#8344,#8345,#8346,#8347,
#8348,#8349,#8350,#8351,#8352,#8353,#8354,#8355,#8356,#8357,#8358,#8359,
#8360,#8361,#8362,#8363,#8364,#8365,#8366,#8367,#8368,#8369,#8370,#8371,
#8372,#8373,#8374,#8375,#8376,#8377,#8378,#8379,#8380,#8381,#8382,#8383,
#8384,#8385,#8386,#8387,#8388,#8389,#8390,#8391,#8392,#8393,#8394,#8395,
#8396,#8397),.UNSPECIFIED.,.F.,.F.,(4,2,2,2,2,2,2,2,2,2,2,2,2,2,2,2,2,2,
2,2,2,2,2,2,2,2,2,2,2,2,2,2,2,2,2,2,2,2,2,2,2,2,2,2,2,2,2,2,2,2,2,2,2,2,
2,2,2,2,2,2,2,2,2,2,2,2,2,2,2,2,2,2,2,2,2,2,2,2,2,2,2,2,2,2,2,2,2,2,2,2,
2,2,2,2,2,2,2,2,2,2,2,2,2,2,2,2,2,2,2,2,2,2,2,2,2,2,2,2,2,2,2,2,2,4),(-1.25725532263633,
-1.23414987783727,-1.229582938354,-1.22660499029235,-1.22419218275367,-1.22142032694857,
-1.21659355295292,-1.19403638234211,-1.16356267873069,-1.14684193795938,
-1.13086079136935,-1.1280953441515,-1.12637067869447,-1.1250169843593,-1.12342393274782,
-1.12050586488755,-1.10449267839333,-1.05290595323384,-1.03438806215691,
-1.02968593302645,-1.02691437014545,-1.02450176742656,-1.02152400798811,
-1.01572012717816,-0.975097572081584,-0.934084235610777,-0.929497593314563,
-0.927722029214994,-0.92644416513048,-0.925046445025526,-0.923025794801693,
-0.917747318444877,-0.90984680205646,-0.883443089779648,-0.839524782096024,
-0.832156197130007,-0.829158726567774,-0.826909172443318,-0.824424342985893,
-0.820941795960919,-0.812336419873437,-0.767823796079561,-0.735297838688778,
-0.730395453104543,-0.728376191473371,-0.72699259471416,-0.725542786094121,
-0.723276191185997,-0.716138950189172,-0.704166476090038,-0.67621647774181,
-0.637112767106812,-0.632241676356427,-0.62917127796705,-0.626750334629781,
-0.62403984157517,-0.619493893030351,-0.601229605733001,-0.562645117989373,
-0.53365581852347,-0.530363377467649,-0.528670057209901,-0.527318133825508,
-0.525699967166895,-0.522664279732112,-0.503681980369015,-0.464405504947726,
-0.437611653226557,-0.432903093952549,-0.429881872289105,-0.427465667883303,
-0.424724169948025,-0.420036768738303,-0.399766309704602,-0.350766018860153,
-0.33406139897186,-0.331265007398607,-0.32953095378834,-0.32817641867556,
-0.326589973665461,-0.32370309643189,-0.308361968464629,-0.26281376606529,
-0.238262921183173,-0.23361333728499,-0.230610029093004,-0.228195242692369,
-0.228148430478243,-0.228105290782643,-0.228065527609278,-0.228028869431055,
-0.227995067192375,-0.227963892453147,-0.227935135657683,-0.227908604541952,
-0.227884122668304,-0.227861528076439,-0.227840672040996,-0.227821417961429,
-0.227803640321601,-0.227775150263939,-0.227747146325044,-0.224871621810508,
-0.219483355561745,-0.212679848683744,-0.197426353486088,-0.162035331886598,
-0.135232805453285,-0.131941228664079,-0.130248061056178,-0.128896102313303,
-0.12727770576582,-0.124241083327297,-0.105233847404728,-0.0640561896920884,
-0.0479072784389079,-0.0368063663789557,-0.0328382139608077,-0.0305122514720755,
-0.0281761756576672,-0.0258175242526361,-0.022775380510453,-0.0147912373815069,
-0.000585061145730822),.UNSPECIFIED.);
#83=B_SPLINE_CURVE_WITH_KNOTS('',3,(#8402,#8403,#8404,#8405,#8406,#8407,
#8408,#8409,#8410,#8411,#8412,#8413,#8414,#8415,#8416,#8417,#8418,#8419,
#8420,#8421,#8422,#8423,#8424,#8425,#8426,#8427,#8428,#8429,#8430,#8431,
#8432,#8433,#8434,#8435,#8436,#8437,#8438,#8439,#8440,#8441,#8442,#8443,
#8444,#8445,#8446,#8447,#8448,#8449,#8450,#8451,#8452,#8453,#8454,#8455,
#8456,#8457,#8458,#8459,#8460,#8461,#8462,#8463,#8464,#8465,#8466,#8467,
#8468,#8469,#8470,#8471,#8472,#8473,#8474,#8475,#8476,#8477,#8478,#8479,
#8480,#8481,#8482,#8483,#8484,#8485,#8486,#8487,#8488,#8489,#8490,#8491,
#8492,#8493,#8494,#8495,#8496,#8497,#8498,#8499,#8500,#8501,#8502,#8503,
#8504,#8505,#8506,#8507,#8508,#8509,#8510,#8511,#8512,#8513,#8514,#8515,
#8516,#8517,#8518,#8519,#8520,#8521,#8522,#8523,#8524,#8525,#8526,#8527,
#8528,#8529,#8530,#8531,#8532,#8533,#8534,#8535,#8536,#8537,#8538,#8539,
#8540,#8541,#8542,#8543,#8544,#8545,#8546,#8547,#8548,#8549,#8550,#8551,
#8552,#8553,#8554,#8555,#8556,#8557,#8558,#8559,#8560,#8561,#8562,#8563,
#8564,#8565,#8566,#8567,#8568,#8569,#8570,#8571,#8572,#8573,#8574,#8575,
#8576,#8577,#8578,#8579,#8580,#8581,#8582,#8583,#8584,#8585,#8586,#8587,
#8588,#8589,#8590,#8591,#8592,#8593,#8594,#8595,#8596,#8597,#8598,#8599,
#8600,#8601,#8602,#8603,#8604,#8605,#8606,#8607,#8608,#8609,#8610,#8611,
#8612,#8613,#8614,#8615,#8616,#8617),.UNSPECIFIED.,.F.,.F.,(4,2,2,2,2,2,
2,2,2,2,2,2,2,2,2,2,2,2,2,2,2,2,2,2,2,2,2,2,2,2,2,2,2,2,2,2,2,2,2,2,2,2,
2,2,2,2,2,2,2,2,2,2,2,2,2,2,2,2,2,2,2,2,2,2,2,2,2,2,2,2,2,2,2,2,2,2,2,2,
2,2,2,2,2,2,2,2,2,2,2,2,2,2,2,2,2,2,2,2,2,2,2,2,2,2,2,2,2,4),(-1.25706550838262,
-1.25688504802724,-1.22123092182879,-1.20728198578521,-1.20462145682404,
-1.20292864050153,-1.20157693858103,-1.19995882124868,-1.19692264692035,
-1.17791534092071,-1.13848753000333,-1.11187309040359,-1.10717132592824,
-1.10415241997231,-1.10173675366566,-1.09899445318844,-1.09430215089612,
-1.07394897361652,-1.02437941311237,-1.00829779650752,-1.00552810482319,
-1.00380220346361,-1.0024484755008,-1.0008564788184,-0.997943117849524,
-0.982031177150865,-0.931454519873525,-0.911951694111017,-0.907181187104882,
-0.904394051993041,-0.901982833889149,-0.899025790607165,-0.893323025750843,
-0.855748344084509,-0.814652098577032,-0.807711750656776,-0.805388647467649,
-0.804071835323865,-0.802700272531822,-0.800825870699864,-0.796454357758817,
-0.776269068168181,-0.725858543838252,-0.711806103004129,-0.707471542862481,
-0.70480766740214,-0.70237671926059,-0.699220907939881,-0.692506507140974,
-0.66598923864767,-0.633486721974839,-0.610250071281972,-0.607000259638474,
-0.605316231189555,-0.603964846583364,-0.602339073773635,-0.599266716608962,
-0.579150978200645,-0.534395181408312,-0.513715621137475,-0.508864325751391,
-0.50605879206878,-0.503648773141945,-0.500714655762829,-0.495123115488161,
-0.450593245270213,-0.413397349567453,-0.408621352095307,-0.406819822084488,
-0.405535135100852,-0.404143462590276,-0.402153841902686,-0.39707811517086,
-0.389580256879378,-0.365476514118443,-0.318300598583093,-0.311023999784254,
-0.307800461103658,-0.30535117500284,-0.302741091976463,-0.298652509683195,
-0.28542925721175,-0.237782995101438,-0.211885060370233,-0.208603818969469,
-0.206912965422761,-0.20558617619989,-0.204013310889401,-0.202307704268895,
-0.199621085582844,-0.194404664338341,-0.180842960677011,-0.136438658626752,
-0.11534775604208,-0.110467976958645,-0.107655845400156,-0.105269056898189,
-0.102352661960632,-0.0968471246601189,-0.0541927809219825,-0.0182779878114133,
-0.0109890940378711,-0.00862216554045305,-0.00715023066165515,-0.00586260574610939,
-0.00449433631278169,-0.00256109927198567,-0.000585266250537942),
 .UNSPECIFIED.);
#84=B_SPLINE_CURVE_WITH_KNOTS('',3,(#8618,#8619,#8620,#8621,#8622,#8623,
#8624,#8625,#8626,#8627,#8628,#8629,#8630,#8631,#8632,#8633,#8634,#8635,
#8636,#8637,#8638,#8639,#8640,#8641,#8642,#8643,#8644,#8645,#8646,#8647,
#8648,#8649,#8650,#8651,#8652,#8653,#8654,#8655,#8656,#8657,#8658,#8659,
#8660,#8661,#8662,#8663,#8664,#8665,#8666,#8667,#8668,#8669,#8670,#8671,
#8672,#8673,#8674,#8675,#8676,#8677,#8678,#8679,#8680,#8681,#8682,#8683,
#8684,#8685,#8686,#8687,#8688,#8689,#8690,#8691,#8692,#8693,#8694,#8695,
#8696,#8697,#8698,#8699,#8700,#8701,#8702,#8703,#8704,#8705,#8706,#8707,
#8708,#8709,#8710,#8711,#8712,#8713,#8714,#8715,#8716,#8717,#8718,#8719,
#8720,#8721,#8722,#8723,#8724,#8725,#8726,#8727,#8728,#8729,#8730,#8731,
#8732,#8733,#8734,#8735,#8736,#8737,#8738,#8739,#8740,#8741,#8742,#8743,
#8744,#8745,#8746,#8747,#8748,#8749,#8750,#8751,#8752,#8753,#8754,#8755,
#8756,#8757,#8758,#8759,#8760,#8761,#8762,#8763,#8764,#8765,#8766,#8767,
#8768,#8769,#8770,#8771,#8772,#8773,#8774,#8775,#8776,#8777,#8778,#8779,
#8780,#8781,#8782,#8783,#8784,#8785,#8786,#8787,#8788,#8789,#8790,#8791,
#8792,#8793,#8794,#8795,#8796,#8797,#8798,#8799,#8800,#8801,#8802,#8803,
#8804),.UNSPECIFIED.,.F.,.F.,(4,3,3,3,3,3,3,3,3,3,3,3,3,3,3,3,3,3,3,3,3,
3,3,3,3,3,3,3,3,3,3,3,3,3,3,3,3,3,3,3,3,3,3,3,3,3,3,3,3,3,3,3,3,3,3,3,3,
3,3,3,3,3,4),(47.1238898042299,47.2435633757992,47.3643071377152,47.4759599628827,
47.5809402011763,47.6857634632907,47.7904640358196,47.8950991401544,47.9997043040436,
48.1043150115907,48.2090361436527,48.3138187074791,48.41878217878,48.4720590397033,
48.5770392779971,48.6818625401117,48.7865631126407,48.8911982169756,48.9958033808649,
49.1004140884122,49.2051352204743,49.3099177843008,49.4148812556019,49.4681581165239,
49.5731383548177,49.6779616169323,49.7826621894614,49.8872972937963,49.9919024576857,
50.0965131652331,50.2012342972952,50.3060168611217,50.4109803324229,50.4642571933445,
50.5692374316383,50.6740606937529,50.7787612662819,50.8833963706168,50.9880015345061,
51.0926122420534,51.1973333741155,51.3021159379419,51.407079409243,51.4603562701651,
51.5653365084589,51.6701597705735,51.7748603431025,51.8794954474374,51.9841006113267,
52.088711318874,52.1934324509361,52.2982150147626,52.4031784860637,52.4564553469857,
52.5606956544191,52.666493039488,52.7704553584402,52.8743554984829,52.9782300106044,
53.0854411916958,53.189437381338,53.298256058154,53.40707473497),
 .UNSPECIFIED.);
#85=B_SPLINE_CURVE_WITH_KNOTS('',3,(#8809,#8810,#8811,#8812,#8813,#8814,
#8815,#8816,#8817,#8818,#8819,#8820,#8821,#8822,#8823,#8824,#8825,#8826,
#8827,#8828,#8829,#8830,#8831,#8832,#8833,#8834,#8835,#8836,#8837,#8838,
#8839,#8840,#8841,#8842,#8843,#8844,#8845,#8846,#8847,#8848,#8849,#8850,
#8851,#8852,#8853,#8854,#8855,#8856,#8857,#8858,#8859,#8860,#8861,#8862,
#8863,#8864,#8865,#8866,#8867,#8868,#8869,#8870,#8871,#8872,#8873,#8874,
#8875,#8876,#8877,#8878,#8879,#8880,#8881,#8882,#8883,#8884,#8885,#8886,
#8887,#8888,#8889,#8890,#8891,#8892,#8893,#8894,#8895,#8896,#8897,#8898,
#8899,#8900,#8901,#8902,#8903,#8904,#8905,#8906,#8907,#8908,#8909,#8910,
#8911,#8912,#8913,#8914,#8915,#8916,#8917,#8918,#8919,#8920,#8921,#8922,
#8923,#8924,#8925,#8926,#8927,#8928,#8929,#8930,#8931,#8932,#8933,#8934,
#8935,#8936,#8937,#8938,#8939,#8940,#8941,#8942,#8943,#8944,#8945,#8946,
#8947,#8948,#8949,#8950,#8951,#8952,#8953,#8954,#8955,#8956,#8957,#8958,
#8959,#8960,#8961,#8962,#8963,#8964,#8965,#8966,#8967,#8968,#8969,#8970,
#8971,#8972,#8973,#8974,#8975,#8976,#8977,#8978,#8979,#8980,#8981,#8982,
#8983,#8984,#8985,#8986,#8987,#8988,#8989,#8990,#8991,#8992,#8993,#8994,
#8995,#8996,#8997,#8998,#8999,#9000,#9001,#9002,#9003,#9004,#9005,#9006,
#9007,#9008,#9009,#9010,#9011,#9012,#9013,#9014,#9015,#9016,#9017,#9018,
#9019,#9020,#9021,#9022,#9023,#9024,#9025,#9026,#9027,#9028),
 .UNSPECIFIED.,.F.,.F.,(4,2,2,2,2,2,2,2,2,2,2,2,2,2,2,2,2,2,2,2,2,2,2,2,
2,2,2,2,2,2,2,2,2,2,2,2,2,2,2,2,2,2,2,2,2,2,2,2,2,2,2,2,2,2,2,2,2,2,2,2,
2,2,2,2,2,2,2,2,2,2,2,2,2,2,2,2,2,2,2,2,2,2,2,2,2,2,2,2,2,2,2,2,2,2,2,2,
2,2,2,2,2,2,2,2,2,2,2,2,2,4),(-2.51349872763998,-2.5038851842131,-2.50087187825048,
-2.4985231050743,-2.49617779550293,-2.49350610377327,-2.48913397617121,
-2.47470867605817,-2.45518971606659,-2.40488695271871,-2.40027525480988,
-2.39836039088578,-2.39698244129476,-2.39567861831703,-2.39341999995963,
-2.38695602689522,-2.34546637603089,-2.31962086310329,-2.30999334617576,
-2.3050613691288,-2.30090026821975,-2.29898551606501,-2.29662411660384,
-2.29381428540162,-2.28894295004069,-2.26813771429483,-2.2234871187881,
-2.20339961855757,-2.20032831136248,-2.19870289031664,-2.1973516768625,
-2.19566771573073,-2.19241762492591,-2.16912071081335,-2.16177742884842,
-2.13115401214413,-2.11533855978587,-2.10496072596096,-2.10121826726596,
-2.09868216334679,-2.09621881385362,-2.09326330676,-2.08584647377472,-2.04087132675203,
-2.01521083977102,-2.00743751507438,-2.00222330775971,-2.00021257853642,
-1.99881697401559,-1.99753726925047,-1.99575417297682,-1.99111527092585,
-1.95126522272148,-1.9096554005371,-1.90382236422733,-1.90083894774715,
-1.8984262730994,-1.89565959200985,-1.89097769849647,-1.87266464531903,
-1.82083654755321,-1.80479767641897,-1.80187859615659,-1.80028543744887,
-1.79893191816085,-1.79720782907602,-1.79444399628042,-1.77849206266062,
-1.76247170689171,-1.76105128892689,-1.72601142173876,-1.71423173734209,
-1.70589529056457,-1.70245605230094,-1.69997940556005,-1.69772181257994,
-1.69411696980672,-1.68735166626761,-1.64455970117892,-1.60965831690555,
-1.603999217502,-1.60192293026968,-1.60051407345145,-1.59924714932525,-1.59718066984107,
-1.59199466371079,-1.53151400501854,-1.50944673885689,-1.504648833987,-1.50188358061218,
-1.49947064558119,-1.49648496376324,-1.49189177919711,-1.46803029563411,
-1.42608797642757,-1.40661575565723,-1.40356387669026,-1.40194246027129,
-1.40059094293453,-1.39890205083461,-1.39562946330555,-1.36564386652456,
-1.32786087722053,-1.30978966882121,-1.30525893783051,-1.30255204688415,
-1.3001308949269,-1.29705556295359,-1.29216722416761,-1.25706550838262),
 .UNSPECIFIED.);
#86=B_SPLINE_CURVE_WITH_KNOTS('',3,(#9029,#9030,#9031,#9032,#9033,#9034,
#9035,#9036,#9037,#9038,#9039),.UNSPECIFIED.,.F.,.F.,(4,1,1,1,1,1,1,1,4),
(53.4070751110265,53.4525544238063,54.4486535006269,55.4447525774475,56.4408516542681,
57.4369507310886,58.4330498079092,59.4291488847298,59.6902577852515),
 .UNSPECIFIED.);
#87=B_SPLINE_CURVE_WITH_KNOTS('',3,(#9044,#9045,#9046,#9047,#9048,#9049,
#9050,#9051,#9052,#9053),.UNSPECIFIED.,.F.,.F.,(4,1,1,1,1,1,1,4),(59.6902663011146,
60.1053097218334,61.101408798654,62.0975078754745,63.0936069522951,64.0897060291157,
65.0858051059363,65.973437039268),.UNSPECIFIED.);
#88=B_SPLINE_CURVE_WITH_KNOTS('',3,(#9054,#9055,#9056,#9057,#9058,#9059,
#9060,#9061,#9062,#9063,#9064,#9065,#9066,#9067,#9068,#9069,#9070,#9071,
#9072,#9073,#9074,#9075,#9076,#9077,#9078,#9079,#9080,#9081,#9082,#9083,
#9084,#9085,#9086,#9087,#9088,#9089,#9090,#9091,#9092,#9093,#9094,#9095,
#9096,#9097,#9098,#9099,#9100,#9101,#9102,#9103,#9104,#9105,#9106,#9107,
#9108,#9109,#9110,#9111,#9112,#9113,#9114,#9115,#9116,#9117,#9118,#9119,
#9120,#9121,#9122,#9123,#9124,#9125,#9126,#9127,#9128,#9129,#9130,#9131,
#9132,#9133,#9134,#9135,#9136,#9137,#9138,#9139,#9140,#9141,#9142,#9143,
#9144,#9145,#9146,#9147,#9148,#9149,#9150,#9151,#9152,#9153,#9154,#9155,
#9156,#9157,#9158,#9159,#9160,#9161,#9162,#9163,#9164,#9165,#9166,#9167,
#9168,#9169,#9170,#9171,#9172,#9173,#9174,#9175,#9176,#9177,#9178,#9179,
#9180,#9181,#9182,#9183,#9184,#9185,#9186,#9187,#9188,#9189,#9190,#9191,
#9192,#9193,#9194,#9195,#9196,#9197,#9198,#9199,#9200,#9201,#9202,#9203,
#9204,#9205,#9206,#9207,#9208,#9209,#9210,#9211,#9212,#9213,#9214,#9215,
#9216,#9217,#9218,#9219,#9220,#9221,#9222,#9223,#9224,#9225,#9226,#9227,
#9228,#9229,#9230,#9231,#9232,#9233,#9234,#9235,#9236,#9237,#9238,#9239,
#9240,#9241,#9242,#9243,#9244,#9245,#9246,#9247,#9248,#9249,#9250,#9251,
#9252,#9253,#9254,#9255,#9256,#9257,#9258,#9259,#9260,#9261,#9262,#9263,
#9264,#9265,#9266,#9267,#9268,#9269,#9270,#9271,#9272,#9273,#9274,#9275,
#9276,#9277,#9278,#9279),.UNSPECIFIED.,.F.,.F.,(4,2,2,2,2,2,2,2,2,2,2,2,
2,2,2,2,2,2,2,2,2,2,2,2,2,2,2,2,2,2,2,2,2,2,2,2,2,2,2,2,2,2,2,2,2,2,2,2,
2,2,2,2,2,2,2,2,2,2,2,2,2,2,2,2,2,2,2,2,2,2,2,2,2,2,2,2,2,2,2,2,2,2,2,2,
2,2,2,2,2,2,2,2,2,2,2,2,2,2,2,2,2,2,2,2,2,2,2,2,2,2,2,2,4),(-2.51352086227721,
-2.47656604450951,-2.47233342613999,-2.46951209352325,-2.46679256411087,
-2.46437402259144,-2.46132081360216,-2.4565050707433,-2.42631519722904,
-2.40240525096532,-2.37761212775579,-2.37031263472917,-2.36859248794638,
-2.36698412358358,-2.36563209473153,-2.36392815619268,-2.36123053290713,
-2.34655872265476,-2.34296884314504,-2.33830237269572,-2.29943217346383,
-2.28363969071847,-2.27667239285055,-2.2711949630713,-2.26825333037283,
-2.26584332268692,-2.26304479523154,-2.25822306675709,-2.23800150479595,
-2.19151157927723,-2.17252446097555,-2.16948910335028,-2.16787126559159,
-2.16651970165235,-2.16482694511829,-2.16153592950984,-2.13288259767781,
-2.09408099352259,-2.07576862879241,-2.07121991123292,-2.06850923027962,
-2.06608902921062,-2.06302080957817,-2.05815560792853,-2.01847891987679,
-1.98830481936321,-1.9731090428728,-1.97022979630961,-1.96864529408586,
-1.96729100790699,-1.96555546778813,-1.96275323033051,-1.94588839017909,
-1.89708562636036,-1.87685173620764,-1.8721677758771,-1.86942751000864,
-1.86701191746648,-1.86399083526381,-1.85928123748612,-1.83243483132589,
-1.79319280498197,-1.77421271403723,-1.7711775920826,-1.76955980174001,
-1.7682082317662,-1.76651541031422,-1.76322410318252,-1.73418596032668,
-1.69568827106528,-1.6774471371647,-1.67290377555124,-1.67019426410786,
-1.66777384515526,-1.66470363304381,-1.65983183381601,-1.62072905144766,
-1.59278533129058,-1.57499486754214,-1.57200297501951,-1.57039434634236,
-1.56904221983833,-1.56733831583323,-1.56464103750746,-1.54997917822018,
-1.5463993725626,-1.53299504820674,-1.50292419740552,-1.48708567683488,
-1.47669680090119,-1.47295279218317,-1.4704163309107,-1.46795316188431,
-1.46499850548168,-1.45758726248084,-1.41255296291875,-1.38693046528234,
-1.37916363718097,-1.37395266080893,-1.37194239682505,-1.37054686165185,
-1.36926701888645,-1.367483463603,-1.36284150830577,-1.32307426153321,-1.2942618662616,
-1.28398035138986,-1.27646816161009,-1.27316789283731,-1.27071554117611,
-1.2684262432894,-1.2652685295823,-1.2571219133552),.UNSPECIFIED.);
#89=B_SPLINE_CURVE_WITH_KNOTS('',3,(#9284,#9285,#9286,#9287,#9288,#9289,
#9290,#9291,#9292,#9293,#9294,#9295,#9296,#9297,#9298,#9299,#9300,#9301,
#9302,#9303,#9304,#9305,#9306,#9307,#9308,#9309,#9310,#9311,#9312,#9313,
#9314,#9315,#9316,#9317,#9318,#9319,#9320,#9321,#9322,#9323,#9324,#9325,
#9326,#9327,#9328,#9329,#9330,#9331,#9332,#9333,#9334,#9335,#9336,#9337,
#9338,#9339,#9340,#9341,#9342,#9343,#9344,#9345,#9346,#9347,#9348,#9349,
#9350,#9351,#9352,#9353,#9354,#9355,#9356,#9357,#9358,#9359,#9360,#9361,
#9362,#9363,#9364,#9365,#9366,#9367,#9368,#9369,#9370,#9371,#9372,#9373,
#9374,#9375,#9376,#9377,#9378,#9379,#9380,#9381,#9382,#9383,#9384,#9385,
#9386,#9387,#9388,#9389,#9390,#9391,#9392,#9393,#9394,#9395,#9396,#9397,
#9398,#9399,#9400,#9401,#9402,#9403,#9404,#9405,#9406,#9407,#9408,#9409,
#9410,#9411,#9412,#9413,#9414,#9415,#9416,#9417,#9418,#9419,#9420,#9421,
#9422,#9423,#9424,#9425,#9426,#9427,#9428,#9429,#9430,#9431,#9432,#9433,
#9434,#9435,#9436,#9437,#9438,#9439,#9440,#9441,#9442,#9443,#9444,#9445,
#9446,#9447,#9448,#9449,#9450,#9451,#9452,#9453,#9454,#9455,#9456,#9457,
#9458,#9459,#9460,#9461,#9462,#9463,#9464,#9465,#9466,#9467,#9468,#9469,
#9470,#9471,#9472,#9473,#9474,#9475,#9476,#9477,#9478,#9479,#9480,#9481,
#9482,#9483,#9484,#9485,#9486,#9487,#9488,#9489,#9490,#9491,#9492,#9493,
#9494,#9495,#9496,#9497,#9498,#9499,#9500,#9501,#9502,#9503,#9504,#9505,
#9506,#9507,#9508,#9509,#9510,#9511,#9512,#9513,#9514,#9515,#9516,#9517,
#9518,#9519,#9520,#9521,#9522,#9523,#9524,#9525,#9526,#9527,#9528,#9529,
#9530,#9531,#9532,#9533,#9534,#9535,#9536,#9537,#9538,#9539,#9540,#9541,
#9542,#9543,#9544,#9545,#9546,#9547,#9548,#9549,#9550,#9551,#9552,#9553,
#9554,#9555,#9556,#9557),.UNSPECIFIED.,.F.,.F.,(4,2,2,2,2,2,2,2,2,2,2,2,
2,2,2,2,2,2,2,2,2,2,2,2,2,2,2,2,2,2,2,2,2,2,2,2,2,2,2,2,2,2,2,2,2,2,2,2,
2,2,2,2,2,2,2,2,2,2,2,2,2,2,2,2,2,2,2,2,2,2,2,2,2,2,2,2,2,2,2,2,2,2,2,2,
2,2,2,2,2,2,2,2,2,2,2,2,2,2,2,2,2,2,2,2,2,2,2,2,2,2,2,2,2,2,2,2,2,2,2,2,
2,2,2,2,2,2,2,2,2,2,2,2,2,2,2,2,4),(-1.25687291994263,-1.25670044137422,
-1.22544272579206,-1.22054547491201,-1.21852746533694,-1.2171444413607,
-1.21569494768325,-1.21342834269509,-1.20628690034842,-1.19430270378767,
-1.16637957239355,-1.1272958187117,-1.12242603417447,-1.11935656334443,
-1.1169364164464,-1.11422688304229,-1.10968270712158,-1.09142792654451,
-1.05287083613732,-1.02387276977237,-1.02058140541397,-1.01888864499246,
-1.01753717185539,-1.01591954804797,-1.0128848895838,-0.993909426007681,
-0.954648925525729,-0.92786077125015,-0.923153668773008,-0.920133419639802,
-0.917718017279809,-0.914977455455784,-0.91029171989732,-0.890029594984095,
-0.841056064952028,-0.824345691015182,-0.821549760239923,-0.819816143281373,
-0.818462048361667,-0.816876234199523,-0.813990793073848,-0.798664597752717,
-0.753209356851707,-0.728538124125303,-0.723910903087646,-0.720914951280207,
-0.718501465016874,-0.715744045447738,-0.71098135724583,-0.689502978810967,
-0.629652331870388,-0.623486184077388,-0.621268664025271,-0.619972782684903,
-0.618589440555912,-0.616644844393399,-0.611853223269203,-0.587515708314427,
-0.584515966709155,-0.53344665596035,-0.52579868490047,-0.522723442859434,
-0.520455039664869,-0.517987806235039,-0.514600566467615,-0.506579705696247,
-0.495380669811647,-0.443561108261493,-0.439734942708405,-0.425651776109235,
-0.422983953027209,-0.421288851084714,-0.419936951411302,-0.418320536155404,
-0.415292749882273,-0.396532325504097,-0.369078749641853,-0.330553627612335,
-0.325677216474872,-0.322605315627897,-0.320184342686376,-0.317475021703886,
-0.312933929526981,-0.294731283787524,-0.256405134860613,-0.227070359910657,
-0.223791774650741,-0.222101486607004,-0.22074977124105,-0.220743834240699,
-0.220737976367287,-0.220732196409144,-0.220726493202849,-0.220720865602647,
-0.220715312474501,-0.220709832678287,-0.220704425161169,-0.220699088817152,
-0.22069382257323,-0.220688625428385,-0.220683496311316,-0.220678434224712,
-0.220673438206272,-0.22066850725514,-0.220663640428295,-0.220658836797703,
-0.220654095435096,-0.220649415408777,-0.220644795845114,-0.220640235867172,
-0.220635734603853,-0.220631291185153,-0.220626904800747,-0.220622574635532,
-0.220618299871072,-0.220613792946687,-0.218962971059349,-0.21573595159757,
-0.211521887709934,-0.16736328941224,-0.131391570959872,-0.126493097899004,
-0.123414585989652,-0.120992935052489,-0.118287569900292,-0.113764372938564,
-0.0957953825526273,-0.0481363765774753,-0.0369810098464935,-0.0267619539712843,
-0.0241129107165841,-0.0225631833115297,-0.0212349036940288,-0.0199043365304187,
-0.0181638814832782,-0.0153923964553053,-0.000584983637756737),
 .UNSPECIFIED.);
#90=B_SPLINE_CURVE_WITH_KNOTS('',3,(#9558,#9559,#9560,#9561,#9562,#9563,
#9564,#9565,#9566,#9567,#9568,#9569,#9570,#9571,#9572,#9573,#9574,#9575,
#9576,#9577,#9578,#9579,#9580,#9581,#9582,#9583,#9584,#9585,#9586,#9587,
#9588,#9589,#9590,#9591,#9592,#9593,#9594,#9595,#9596,#9597,#9598,#9599,
#9600,#9601,#9602,#9603,#9604,#9605,#9606,#9607,#9608,#9609,#9610,#9611,
#9612,#9613,#9614,#9615,#9616,#9617,#9618,#9619,#9620,#9621,#9622,#9623,
#9624,#9625,#9626,#9627,#9628,#9629,#9630,#9631,#9632,#9633,#9634,#9635,
#9636,#9637,#9638,#9639,#9640,#9641,#9642,#9643,#9644,#9645,#9646,#9647,
#9648,#9649,#9650,#9651,#9652,#9653,#9654,#9655,#9656,#9657,#9658,#9659,
#9660,#9661,#9662,#9663,#9664,#9665,#9666,#9667,#9668,#9669,#9670,#9671,
#9672,#9673,#9674,#9675,#9676,#9677,#9678,#9679,#9680,#9681,#9682,#9683,
#9684,#9685,#9686,#9687,#9688,#9689,#9690,#9691,#9692,#9693,#9694,#9695,
#9696,#9697,#9698,#9699,#9700,#9701,#9702,#9703,#9704,#9705,#9706,#9707,
#9708,#9709,#9710,#9711,#9712,#9713,#9714,#9715,#9716,#9717,#9718,#9719,
#9720,#9721,#9722,#9723,#9724,#9725,#9726,#9727,#9728,#9729,#9730,#9731,
#9732,#9733,#9734,#9735,#9736,#9737,#9738,#9739,#9740,#9741,#9742,#9743,
#9744,#9745,#9746,#9747,#9748,#9749,#9750,#9751,#9752,#9753,#9754,#9755,
#9756,#9757,#9758,#9759,#9760,#9761,#9762,#9763,#9764,#9765),
 .UNSPECIFIED.,.F.,.F.,(4,2,2,2,2,2,2,2,2,2,2,2,2,2,2,2,2,2,2,2,2,2,2,2,
2,2,2,2,2,2,2,2,2,2,2,2,2,2,2,2,2,2,2,2,2,2,2,2,2,2,2,2,2,2,2,2,2,2,2,2,
2,2,2,2,2,2,2,2,2,2,2,2,2,2,2,2,2,2,2,2,2,2,2,2,2,2,2,2,2,2,2,2,2,2,2,2,
2,2,2,2,2,2,2,4),(-1.2571219133552,-1.21585553434398,-1.17958221126086,
-1.17476866209243,-1.17296230431759,-1.17167636964021,-1.17028582140703,
-1.16830187538236,-1.16326227083586,-1.15583524974168,-1.13211852174542,
-1.08436975214487,-1.07785825667516,-1.07432096280615,-1.07185080152282,
-1.06932293844234,-1.06562104986835,-1.05553889594932,-1.04033699297451,
-1.00515383303319,-0.978078340918164,-0.974786502194116,-0.973093479460995,
-0.97174178701376,-0.97012388889707,-0.967088684103669,-0.948108602481126,
-0.908833085805069,-0.88205019072271,-0.8773426556386,-0.87432201651327,
-0.871906230061974,-0.869165154845333,-0.86447834789892,-0.844208227024231,
-0.795195708412977,-0.778516233458754,-0.775721247055763,-0.773987767334826,
-0.772633485086136,-0.771047108886636,-0.768159788433407,-0.75280187722704,
-0.707107100110468,-0.682675194869783,-0.678057519106133,-0.675064228541182,
-0.672650590105053,-0.669890488739537,-0.665116772060569,-0.643464742236623,
-0.595369446933154,-0.579266712389494,-0.576496088483726,-0.57476989686073,
-0.573416133958902,-0.571824321383452,-0.56891186755737,-0.553020281595855,
-0.502643427113485,-0.482943300007431,-0.478159281736766,-0.475369040543534,
-0.472958012697656,-0.470004843301442,-0.464321067347851,-0.421209691770432,
-0.382683277144806,-0.377955139881056,-0.376159748323764,-0.374876674193312,
-0.373483608914664,-0.371486814726044,-0.366364850758388,-0.358775871990412,
-0.334166487798117,-0.287728646418363,-0.280398527354053,-0.277456601328946,
-0.274996434646347,-0.27245521803386,-0.268689335682666,-0.258140745358293,
-0.2419635344494,-0.21501066525948,-0.183744437376953,-0.178839697497763,
-0.176820155866155,-0.17543659513459,-0.174016170921965,-0.171906577870583,
-0.169370041189546,-0.164563130168757,-0.152552384296939,-0.127153904817075,
-0.089000505522226,-0.081538242306694,-0.078494506707217,-0.0762338150673216,
-0.0737598363842677,-0.0703355368811069,-0.0620911922644493,-0.0504811963099944,
-0.000709655758544155),.UNSPECIFIED.);
#91=B_SPLINE_CURVE_WITH_KNOTS('',3,(#9770,#9771,#9772,#9773,#9774,#9775,
#9776,#9777,#9778,#9779,#9780,#9781,#9782,#9783,#9784,#9785,#9786,#9787,
#9788,#9789,#9790,#9791,#9792,#9793,#9794,#9795,#9796,#9797,#9798,#9799,
#9800,#9801,#9802,#9803,#9804,#9805,#9806,#9807,#9808,#9809,#9810,#9811,
#9812,#9813,#9814,#9815,#9816,#9817,#9818,#9819,#9820,#9821,#9822,#9823,
#9824,#9825,#9826,#9827,#9828,#9829,#9830,#9831,#9832,#9833,#9834,#9835,
#9836,#9837,#9838,#9839,#9840,#9841,#9842,#9843,#9844,#9845,#9846,#9847,
#9848,#9849,#9850,#9851,#9852,#9853,#9854,#9855,#9856,#9857,#9858,#9859,
#9860,#9861,#9862,#9863,#9864,#9865,#9866,#9867,#9868,#9869,#9870,#9871,
#9872,#9873,#9874,#9875,#9876,#9877,#9878,#9879,#9880,#9881,#9882,#9883,
#9884,#9885,#9886,#9887,#9888,#9889,#9890,#9891,#9892,#9893,#9894,#9895,
#9896,#9897,#9898,#9899,#9900,#9901,#9902,#9903,#9904,#9905,#9906,#9907,
#9908,#9909,#9910,#9911,#9912,#9913,#9914,#9915,#9916,#9917,#9918,#9919,
#9920,#9921,#9922,#9923,#9924,#9925,#9926,#9927,#9928,#9929,#9930,#9931,
#9932,#9933,#9934,#9935,#9936,#9937,#9938,#9939,#9940,#9941,#9942,#9943,
#9944,#9945,#9946,#9947,#9948,#9949,#9950,#9951,#9952,#9953,#9954,#9955,
#9956,#9957,#9958,#9959,#9960,#9961,#9962,#9963,#9964,#9965,#9966,#9967,
#9968,#9969,#9970,#9971,#9972,#9973,#9974,#9975,#9976,#9977,#9978,#9979,
#9980,#9981),.UNSPECIFIED.,.F.,.F.,(4,2,2,2,2,2,2,2,2,2,2,2,2,2,2,2,2,2,
2,2,2,2,2,2,2,2,2,2,2,2,2,2,2,2,2,2,2,2,2,2,2,2,2,2,2,2,2,2,2,2,2,2,2,2,
2,2,2,2,2,2,2,2,2,2,2,2,2,2,2,2,2,2,2,2,2,2,2,2,2,2,2,2,2,2,2,2,2,2,2,2,
2,2,2,2,2,2,2,2,2,2,2,2,2,2,2,4),(-2.51291706895655,-2.51217911276532,-2.51063689552374,
-2.50794325041847,-2.50342063117696,-2.48648490772758,-2.47445369401095,
-2.45120443821324,-2.42765797896785,-2.42026315675441,-2.41524076903387,
-2.41325986478204,-2.41187019828096,-2.41058406938235,-2.40877608965551,
-2.40394754532802,-2.36812421218677,-2.33662758073177,-2.32025626196319,
-2.31586426301344,-2.31358460684056,-2.31122446939816,-2.3084046314995,
-2.30333115754943,-2.27796143210425,-2.23315363221779,-2.21790935496887,
-2.2150280563601,-2.21344325340457,-2.21208922638083,-2.21035468420121,
-2.20755533770113,-2.19075354860527,-2.14190215917196,-2.12166273652728,
-2.1169789055173,-2.11423892095307,-2.11182370065366,-2.10880324812348,
-2.10409495063136,-2.07727006120171,-2.03801802718977,-2.01903793102046,
-2.01600315993614,-2.01438558761069,-2.01303421787631,-2.0113416699841,
-2.00805096034691,-1.97910582934848,-1.94054369442165,-1.92228873755923,
-1.91774479976322,-1.91503541459223,-1.91261540171038,-1.90954610355304,
-1.90467655375541,-1.86554768152715,-1.83752767537584,-1.81984233534287,
-1.81685483750885,-1.81524728711971,-1.81389530275413,-1.81219061018443,
-1.8094902995344,-1.79476215056747,-1.74396224471499,-1.72344061151146,
-1.71873842379443,-1.71599445773844,-1.71357979721617,-1.71056540439297,
-1.70587692922607,-1.67968717862693,-1.6356440025421,-1.62050060664471,
-1.61762425451455,-1.61604052395961,-1.61468638491076,-1.61295037187428,
-1.61014609782504,-1.59322291945917,-1.54448364740929,-1.52426141513679,
-1.51957873469804,-1.51683901057391,-1.5144237704685,-1.5114029637783,-1.50669347457347,
-1.47983348713225,-1.44061332355789,-1.42163894350217,-1.41860438167521,
-1.41698685879972,-1.41563549413268,-1.41394290704103,-1.41065198991999,
-1.38341844914667,-1.34842121518167,-1.33324218259898,-1.32317072898436,
-1.31947086396263,-1.31694381191842,-1.31447400006986,-1.31093643446459,
-1.30442234628972,-1.25687291994263),.UNSPECIFIED.);
#92=B_SPLINE_CURVE_WITH_KNOTS('',3,(#9983,#9984,#9985,#9986),
 .UNSPECIFIED.,.F.,.F.,(4,4),(-0.000709655758544155,-0.000586166170592014),
 .UNSPECIFIED.);
#93=B_SPLINE_CURVE_WITH_KNOTS('',3,(#9987,#9988,#9989,#9990,#9991,#9992,
#9993,#9994,#9995,#9996,#9997,#9998,#9999,#10000,#10001,#10002,#10003,#10004,
#10005,#10006,#10007,#10008,#10009,#10010,#10011,#10012,#10013,#10014,#10015,
#10016,#10017,#10018,#10019,#10020,#10021,#10022,#10023,#10024,#10025,#10026,
#10027,#10028,#10029,#10030,#10031,#10032,#10033,#10034,#10035,#10036,#10037,
#10038,#10039,#10040,#10041,#10042,#10043,#10044,#10045,#10046,#10047,#10048,
#10049,#10050,#10051,#10052,#10053,#10054,#10055,#10056,#10057,#10058,#10059,
#10060,#10061,#10062,#10063,#10064,#10065,#10066,#10067,#10068,#10069,#10070,
#10071,#10072,#10073,#10074,#10075,#10076,#10077,#10078,#10079,#10080,#10081,
#10082,#10083,#10084,#10085,#10086,#10087,#10088,#10089,#10090,#10091,#10092,
#10093,#10094,#10095,#10096,#10097,#10098,#10099,#10100,#10101,#10102,#10103,
#10104,#10105,#10106,#10107,#10108,#10109,#10110,#10111,#10112,#10113,#10114,
#10115,#10116,#10117,#10118,#10119,#10120,#10121,#10122,#10123,#10124,#10125,
#10126,#10127,#10128,#10129,#10130,#10131,#10132,#10133,#10134,#10135,#10136,
#10137,#10138,#10139,#10140,#10141,#10142,#10143,#10144,#10145,#10146,#10147,
#10148,#10149,#10150,#10151,#10152,#10153,#10154,#10155,#10156,#10157,#10158,
#10159,#10160,#10161,#10162,#10163,#10164,#10165,#10166,#10167,#10168,#10169,
#10170,#10171,#10172,#10173,#10174,#10175,#10176,#10177,#10178,#10179,#10180,
#10181,#10182,#10183,#10184,#10185,#10186,#10187,#10188,#10189,#10190,#10191,
#10192,#10193,#10194,#10195,#10196,#10197,#10198,#10199,#10200,#10201,#10202,
#10203,#10204,#10205,#10206,#10207,#10208,#10209,#10210,#10211,#10212,#10213,
#10214,#10215,#10216,#10217,#10218,#10219,#10220,#10221,#10222,#10223,#10224,
#10225,#10226,#10227,#10228,#10229,#10230,#10231,#10232,#10233,#10234,#10235,
#10236,#10237,#10238,#10239,#10240,#10241,#10242,#10243,#10244,#10245,#10246,
#10247,#10248,#10249,#10250,#10251,#10252,#10253,#10254,#10255,#10256),
 .UNSPECIFIED.,.F.,.F.,(4,2,2,2,2,2,2,2,2,2,2,2,2,2,2,2,2,2,2,2,2,2,2,2,
2,2,2,2,2,2,2,2,2,2,2,2,2,2,2,2,2,2,2,2,2,2,2,2,2,2,2,2,2,2,2,2,2,2,2,2,
2,2,2,2,2,2,2,2,2,2,2,2,2,2,2,2,2,2,2,2,2,2,2,2,2,2,2,2,2,2,2,2,2,2,2,2,
2,2,2,2,2,2,2,2,2,2,2,2,2,2,2,2,2,2,2,2,2,2,2,2,2,2,2,2,2,2,2,2,2,2,2,2,
2,2,4),(-2.51330268493464,-2.49556538564027,-2.49290201701533,-2.49120615253485,
-2.4898904663098,-2.48853737825745,-2.4869430300399,-2.48409762702869,-2.47128896680276,
-2.4594856886688,-2.41535605773799,-2.39751294833082,-2.39300046458648,
-2.39029794958568,-2.38787661178151,-2.38479543541319,-2.37988650000792,
-2.34346083290876,-2.29973097890562,-2.2955324927909,-2.29231687940625,
-2.29066783875272,-2.29066333181592,-2.29065904753134,-2.29065470789311,
-2.29065031212376,-2.29064585936457,-2.29064134876928,-2.29063677950006,
-2.29063215069075,-2.2906274614583,-2.29062271091419,-2.29061789813152,
-2.29061302220024,-2.29060808215181,-2.29060307702415,-2.29059800585755,
-2.29059286764328,-2.29058766135885,-2.29058238598007,-2.29057704046294,
-2.29057162376439,-2.29056613477796,-2.29056057237955,-2.29055493547149,
-2.28920394315063,-2.28752444821789,-2.28429479280678,-2.26299202177995,
-2.21815865601418,-2.19859242037314,-2.19395368985072,-2.19122342722089,
-2.18880662601149,-2.18577070035647,-2.18101189096847,-2.15267573831262,
-2.10132969685269,-2.09673666984598,-2.09325352969231,-2.09154386244977,
-2.09032098791343,-2.08876905430401,-2.08610960623211,-2.07576791518943,
-2.03742639767992,-2.01267364675829,-1.99854453057771,-1.99436137395314,
-1.99173088340836,-1.98928993708555,-1.9861167451348,-1.97938067267917,
-1.92770112872361,-1.89770629831308,-1.89412719200211,-1.89239855426219,
-1.89104472591207,-1.88945499836791,-1.88663076507916,-1.87414733007131,
-1.86582787793111,-1.82729010527406,-1.80980727117441,-1.8023400237277,
-1.79648929718897,-1.79350214854313,-1.7910890279511,-1.78832465873778,
-1.78365345231183,-1.76548722313976,-1.75741552951203,-1.71264751446029,
-1.69740586177275,-1.69452411190569,-1.69293895079597,-1.69158454927969,
-1.68984943899942,-1.68704900584593,-1.67023467053815,-1.62137744018325,
-1.60113366444254,-1.59644863952822,-1.59370792931997,-1.59129205293021,
-1.58827075816209,-1.58356110556567,-1.55672662334708,-1.51746606820367,
-1.49848120852406,-1.49544562871142,-1.49382762115934,-1.49247588538718,
-1.49078287596293,-1.48749126010249,-1.45852444750407,-1.41996282294013,
-1.40170550035024,-1.39716052662444,-1.39445045047062,-1.39202977465648,
-1.38895957347952,-1.38408846633085,-1.34495437080746,-1.31694045752379,
-1.29923291579913,-1.29624393479665,-1.29463580566202,-1.29328346506894,
-1.29157848856973,-1.28887803285747,-1.27415762286202,-1.27008168493941,
-1.25730851664327,-1.25713482558798),.UNSPECIFIED.);
#94=B_SPLINE_CURVE_WITH_KNOTS('',3,(#10261,#10262,#10263,#10264,#10265,
#10266,#10267,#10268,#10269,#10270,#10271,#10272,#10273,#10274,#10275,#10276,
#10277,#10278,#10279,#10280,#10281,#10282,#10283,#10284,#10285,#10286,#10287,
#10288,#10289,#10290,#10291,#10292,#10293,#10294,#10295,#10296,#10297,#10298,
#10299,#10300,#10301,#10302,#10303,#10304,#10305,#10306,#10307,#10308,#10309,
#10310,#10311,#10312,#10313,#10314,#10315,#10316,#10317,#10318,#10319,#10320,
#10321,#10322,#10323,#10324,#10325,#10326,#10327,#10328,#10329,#10330,#10331,
#10332,#10333,#10334,#10335,#10336,#10337,#10338,#10339,#10340,#10341,#10342,
#10343,#10344,#10345,#10346,#10347,#10348,#10349,#10350,#10351,#10352,#10353,
#10354,#10355,#10356,#10357,#10358,#10359,#10360,#10361,#10362,#10363,#10364,
#10365,#10366,#10367,#10368,#10369,#10370,#10371,#10372,#10373,#10374,#10375,
#10376,#10377,#10378,#10379,#10380,#10381,#10382,#10383,#10384,#10385,#10386,
#10387,#10388,#10389,#10390,#10391,#10392,#10393,#10394,#10395,#10396,#10397,
#10398,#10399,#10400,#10401,#10402,#10403,#10404,#10405,#10406,#10407,#10408,
#10409,#10410,#10411,#10412,#10413,#10414,#10415,#10416,#10417,#10418,#10419,
#10420,#10421,#10422,#10423,#10424,#10425,#10426,#10427,#10428,#10429,#10430,
#10431,#10432,#10433,#10434,#10435,#10436,#10437,#10438,#10439,#10440,#10441,
#10442,#10443,#10444,#10445,#10446,#10447,#10448,#10449,#10450,#10451,#10452,
#10453,#10454,#10455,#10456,#10457,#10458,#10459,#10460,#10461,#10462,#10463,
#10464,#10465,#10466,#10467,#10468,#10469,#10470),.UNSPECIFIED.,.F.,.F.,
(4,2,2,2,2,2,2,2,2,2,2,2,2,2,2,2,2,2,2,2,2,2,2,2,2,2,2,2,2,2,2,2,2,2,2,
2,2,2,2,2,2,2,2,2,2,2,2,2,2,2,2,2,2,2,2,2,2,2,2,2,2,2,2,2,2,2,2,2,2,2,2,
2,2,2,2,2,2,2,2,2,2,2,2,2,2,2,2,2,2,2,2,2,2,2,2,2,2,2,2,2,2,2,2,2,4),(-1.25709415659235,
-1.20640776434646,-1.19949059973977,-1.19633157902701,-1.19389272663439,
-1.19125577253466,-1.18704341112428,-1.17262444675379,-1.14707136650296,
-1.1065532048592,-1.0989463085716,-1.09653949245647,-1.09505883103481,-1.09367705061084,
-1.09174094581927,-1.08700122647073,-1.06320431902338,-1.0468965029411,
-1.00825510778017,-1.00081720987613,-0.997777743550822,-0.99551817125555,
-0.993043409768709,-0.989614315921719,-0.981340028934202,-0.96967436851556,
-0.935260274475562,-0.903870373890439,-0.898972581023899,-0.896954239251892,
-0.895570951648383,-0.894121145694341,-0.891853989000944,-0.884710282026987,
-0.872721694792077,-0.844795173472053,-0.805704450672145,-0.80083364696165,
-0.797763547326173,-0.795342913126938,-0.79263284301255,-0.788087788236677,
-0.769829787890545,-0.731266848868859,-0.702260562142043,-0.698968534151507,
-0.697275433236117,-0.695923688692776,-0.69430574055331,-0.691270475048001,
-0.672291268862101,-0.633023266047516,-0.606229308241835,-0.601521245865389,
-0.598500385783588,-0.596084498009793,-0.593343388847281,-0.588656726000295,
-0.568390739487646,-0.519408740892965,-0.502693531983316,-0.49989697825667,
-0.49816299474903,-0.496808626469107,-0.49522250722303,-0.49233654860809,
-0.477008557221062,-0.431554319187296,-0.406867501217787,-0.402238904143188,
-0.399242214145966,-0.39682823271113,-0.394070355926535,-0.389307154268813,
-0.367831769146908,-0.308068269781723,-0.301817978401269,-0.299588658040684,
-0.298290284251489,-0.296908136839533,-0.294971429070456,-0.290229799167671,
-0.266419438403095,-0.259752200029668,-0.210724612084919,-0.203759203931526,
-0.200539388065986,-0.198131362322505,-0.19587147663332,-0.192184896994095,
-0.182215643775771,-0.167247038458566,-0.134373466722911,-0.104590994909892,
-0.101295954150854,-0.0996020247622997,-0.0982500068753463,-0.0966321943319972,
-0.0935984249278762,-0.0746754017447715,-0.029992239982236,-0.00898602795741176,
-0.0040113896938448,-0.00182984320022838,-0.000585605296785841),
 .UNSPECIFIED.);
#95=B_SPLINE_CURVE_WITH_KNOTS('',3,(#10471,#10472,#10473,#10474,#10475,
#10476,#10477,#10478,#10479,#10480,#10481,#10482,#10483,#10484,#10485,#10486,
#10487,#10488,#10489,#10490,#10491,#10492,#10493,#10494,#10495,#10496,#10497,
#10498,#10499,#10500,#10501,#10502,#10503,#10504,#10505,#10506,#10507,#10508,
#10509,#10510,#10511,#10512,#10513,#10514,#10515,#10516,#10517,#10518,#10519,
#10520,#10521,#10522,#10523,#10524,#10525,#10526,#10527,#10528,#10529,#10530,
#10531,#10532,#10533,#10534,#10535,#10536,#10537,#10538,#10539,#10540,#10541,
#10542,#10543,#10544,#10545,#10546,#10547,#10548,#10549,#10550,#10551,#10552,
#10553,#10554,#10555,#10556,#10557,#10558,#10559,#10560,#10561,#10562,#10563,
#10564,#10565,#10566,#10567,#10568,#10569,#10570,#10571,#10572,#10573,#10574,
#10575,#10576,#10577,#10578,#10579,#10580,#10581,#10582,#10583,#10584,#10585,
#10586,#10587,#10588,#10589,#10590,#10591,#10592,#10593,#10594,#10595,#10596,
#10597,#10598,#10599,#10600,#10601,#10602,#10603,#10604,#10605,#10606,#10607,
#10608,#10609,#10610,#10611,#10612,#10613,#10614,#10615,#10616,#10617,#10618,
#10619,#10620,#10621,#10622,#10623,#10624,#10625,#10626,#10627,#10628,#10629,
#10630,#10631,#10632,#10633,#10634,#10635,#10636,#10637,#10638,#10639,#10640,
#10641,#10642,#10643,#10644,#10645,#10646,#10647,#10648,#10649,#10650,#10651,
#10652,#10653,#10654,#10655,#10656,#10657,#10658,#10659,#10660,#10661,#10662,
#10663,#10664,#10665,#10666,#10667,#10668,#10669,#10670,#10671,#10672,#10673,
#10674,#10675,#10676,#10677,#10678,#10679,#10680,#10681,#10682),
 .UNSPECIFIED.,.F.,.F.,(4,2,2,2,2,2,2,2,2,2,2,2,2,2,2,2,2,2,2,2,2,2,2,2,
2,2,2,2,2,2,2,2,2,2,2,2,2,2,2,2,2,2,2,2,2,2,2,2,2,2,2,2,2,2,2,2,2,2,2,2,
2,2,2,2,2,2,2,2,2,2,2,2,2,2,2,2,2,2,2,2,2,2,2,2,2,2,2,2,2,2,2,2,2,2,2,2,
2,2,2,2,2,2,2,2,2,4),(-1.25713482558798,-1.20644675376907,-1.1995293594853,
-1.19637023363597,-1.19393129996726,-1.19129425787816,-1.18708175565679,
-1.17266230639527,-1.14710836121802,-1.10658880303566,-1.09898171941286,
-1.09657483108271,-1.09509412208213,-1.09371229474114,-1.09177612057331,
-1.08703621356417,-1.06323820447604,-1.04693474455628,-1.00828721555779,
-1.00084927521382,-0.997809742935599,-0.995550104004087,-0.993075252294618,
-0.989646001541223,-0.981371177480144,-0.969704643406962,-0.935286777321501,
-0.903899327022173,-0.899001370195921,-0.896982961051145,-0.895599627333541,
-0.894149773094077,-0.891882540955324,-0.88473859671137,-0.872749611529297,
-0.844822165952047,-0.805730149644355,-0.800859183940215,-0.79778898210454,
-0.795368267259881,-0.792658106784467,-0.788112900276069,-0.769854287050508,
-0.731290039031209,-0.702282832824227,-0.698990695394506,-0.697297538120897,
-0.695945748538126,-0.694327746417834,-0.691292379434596,-0.672312529542336,
-0.633043143986475,-0.606248391037856,-0.601540175329844,-0.598519215674788,
-0.596103247498412,-0.593362046277113,-0.58867522393931,-0.568408510601516,
-0.519424527871355,-0.502709158298285,-0.499912527923449,-0.498178491595468,
-0.496824078577472,-0.495237902870162,-0.492351831340346,-0.477022981814089,
-0.431564473403236,-0.406879740383813,-0.402251111410569,-0.399254358957876,
-0.396840299974115,-0.394082304881359,-0.389318823240375,-0.367840721263265,
-0.308048120815742,-0.301820309537888,-0.299594023689091,-0.298296218232952,
-0.296913626833427,-0.294974606703214,-0.290219023402518,-0.266264641273261,
-0.26219170805801,-0.210233333209888,-0.203584032415346,-0.2004266854532,
-0.198029171265855,-0.195770583917539,-0.192007638571533,-0.181483716850691,
-0.165359799630568,-0.138322430870117,-0.107032303177929,-0.102133213625417,
-0.100114413239973,-0.0987308363359355,-0.0972807521829198,-0.0950132045020056,
-0.087868631250021,-0.0758790001103155,-0.0312122114974481,-0.00918919760743087,
-0.00408090742722382,-0.00185725317603439,-0.000585604919035816),
 .UNSPECIFIED.);
#96=B_SPLINE_CURVE_WITH_KNOTS('',3,(#10688,#10689,#10690,#10691),
 .UNSPECIFIED.,.F.,.F.,(4,4),(-0.000709656257275801,-0.000586166555388535),
 .UNSPECIFIED.);
#97=B_SPLINE_CURVE_WITH_KNOTS('',3,(#10692,#10693,#10694,#10695,#10696,
#10697,#10698,#10699,#10700,#10701,#10702,#10703,#10704,#10705,#10706,#10707,
#10708,#10709,#10710,#10711,#10712,#10713,#10714,#10715,#10716,#10717,#10718,
#10719,#10720,#10721,#10722,#10723,#10724,#10725,#10726,#10727,#10728,#10729,
#10730,#10731,#10732,#10733,#10734,#10735,#10736,#10737,#10738,#10739,#10740,
#10741,#10742,#10743,#10744,#10745,#10746,#10747,#10748,#10749,#10750,#10751,
#10752,#10753,#10754,#10755,#10756,#10757,#10758,#10759,#10760,#10761,#10762,
#10763,#10764,#10765,#10766,#10767,#10768,#10769,#10770,#10771,#10772,#10773,
#10774,#10775,#10776,#10777,#10778,#10779,#10780,#10781,#10782,#10783,#10784,
#10785,#10786,#10787,#10788,#10789,#10790,#10791,#10792,#10793,#10794,#10795,
#10796,#10797,#10798,#10799,#10800,#10801,#10802,#10803,#10804,#10805,#10806,
#10807,#10808,#10809,#10810,#10811,#10812,#10813,#10814,#10815,#10816,#10817,
#10818,#10819,#10820,#10821,#10822,#10823,#10824,#10825,#10826,#10827,#10828,
#10829,#10830,#10831,#10832,#10833,#10834,#10835,#10836,#10837,#10838,#10839,
#10840,#10841,#10842,#10843,#10844,#10845,#10846,#10847,#10848,#10849,#10850,
#10851,#10852,#10853,#10854,#10855,#10856,#10857,#10858,#10859,#10860,#10861,
#10862,#10863,#10864,#10865,#10866,#10867,#10868,#10869,#10870,#10871,#10872,
#10873,#10874,#10875,#10876,#10877,#10878,#10879,#10880,#10881,#10882,#10883,
#10884,#10885,#10886,#10887,#10888,#10889,#10890,#10891,#10892,#10893,#10894,
#10895,#10896,#10897,#10898,#10899,#10900,#10901,#10902,#10903,#10904,#10905,
#10906,#10907,#10908,#10909,#10910,#10911,#10912,#10913,#10914,#10915,#10916,
#10917,#10918,#10919,#10920,#10921,#10922,#10923,#10924,#10925,#10926,#10927,
#10928,#10929,#10930,#10931,#10932,#10933,#10934,#10935,#10936,#10937,#10938,
#10939,#10940,#10941,#10942,#10943,#10944,#10945,#10946,#10947,#10948,#10949,
#10950,#10951,#10952,#10953,#10954,#10955,#10956,#10957,#10958,#10959,#10960,
#10961,#10962,#10963,#10964,#10965,#10966,#10967,#10968,#10969,#10970,#10971,
#10972,#10973,#10974,#10975,#10976,#10977,#10978,#10979),.UNSPECIFIED.,
 .F.,.F.,(4,2,2,2,2,2,2,2,2,2,2,2,2,2,2,2,2,2,2,2,2,2,2,2,2,2,2,2,2,2,2,
2,2,2,2,2,2,2,2,2,2,2,2,2,2,2,2,2,2,2,2,2,2,2,2,2,2,2,2,2,2,2,2,2,2,2,2,
2,2,2,2,2,2,2,2,2,2,2,2,2,2,2,2,2,2,2,2,2,2,2,2,2,2,2,2,2,2,2,2,2,2,2,2,
2,2,2,2,2,2,2,2,2,2,2,2,2,2,2,2,2,2,2,2,2,2,2,2,2,2,2,2,2,2,2,2,2,2,2,2,
2,2,2,2,4),(-2.513227510422,-2.49549100342488,-2.49282775470627,-2.49113196652391,
-2.48981633945341,-2.48846331221699,-2.48686903560395,-2.48402376026985,
-2.47121567323448,-2.45941292655917,-2.41532654529159,-2.39744834645147,
-2.39293328263591,-2.39023027791097,-2.38780916465,-2.38472918193759,-2.37982397991019,
-2.34351958773065,-2.29967371101752,-2.29547121444927,-2.29225318682126,
-2.29060369057569,-2.29059918669318,-2.29059491656758,-2.29059059130032,
-2.29058621008268,-2.2905817721001,-2.29057727652477,-2.29057272250903,
-2.2905681091623,-2.29056343561767,-2.29055870099257,-2.29055390437244,
-2.29054904483257,-2.29054412142136,-2.29053913318046,-2.29053407916612,
-2.2905289583675,-2.29052376976824,-2.29051851233955,-2.2905131850438,-2.29050778680207,
-2.2905023165664,-2.29049677322567,-2.2904911556495,-2.29048546270861,-2.29047969324334,
-2.29047384609186,-2.2904679200371,-2.29046191386199,-2.29045582631849,
-2.2904496561538,-2.2904434020707,-2.28909144987658,-2.28738802560439,-2.28469198556758,
-2.27005015595464,-2.26571145215248,-2.23001093200308,-2.20224342815924,
-2.19537099996554,-2.19218615081721,-2.18975169922929,-2.18710257091817,
-2.18283345204478,-2.16934355302114,-2.11226828181438,-2.09578216400288,
-2.09284344045,-2.09124613476314,-2.08989309562249,-2.08817473138067,-2.08542970579341,
-2.06978975619767,-2.05361936028148,-2.02381675878906,-2.00796735620891,
-1.99757322460325,-1.99382843870656,-1.99129176904384,-1.98882863975991,
-1.98587432199708,-1.9784655127671,-1.93332593671369,-1.90778017751212,
-1.90002654650968,-1.89482215648459,-1.89281286038972,-1.89141748566302,
-1.89013738325237,-1.88835292768879,-1.88370483978494,-1.84410029648695,
-1.80226415702097,-1.79642417589041,-1.79343926464616,-1.7910263780879,
-1.78826054926734,-1.78358272938012,-1.76532655909163,-1.75735536328343,
-1.71259138206219,-1.69735056706792,-1.69446892929207,-1.69288382448007,
-1.69152946773313,-1.689794410528,-1.68699405482629,-1.67017989429762,-1.62132463450118,
-1.60108158385312,-1.59639671836579,-1.59365610022755,-1.59124030427927,
-1.5882191091709,-1.58350961011462,-1.5566759269351,-1.5174167529684,-1.49843253711033,
-1.49539705882048,-1.49377910527363,-1.49242741456157,-1.49073446152159,
-1.48744295515195,-1.45847707440362,-1.41991674893802,-1.40166003702122,
-1.39711521490905,-1.39440522911728,-1.39198463399448,-1.38891453513705,
-1.38404359029518,-1.34491078530148,-1.31689778684609,-1.29919084942543,
-1.29620196856318,-1.29459389314123,-1.29324159762496,-1.29153667786007,
-1.28883631183996,-1.27411638686656,-1.27004059496124,-1.2572678417837,
-1.25709415659235),.UNSPECIFIED.);
#98=B_SPLINE_CURVE_WITH_KNOTS('',3,(#10980,#10981,#10982,#10983,#10984,
#10985,#10986,#10987,#10988,#10989,#10990,#10991,#10992,#10993,#10994,#10995,
#10996,#10997,#10998,#10999,#11000,#11001,#11002,#11003,#11004,#11005,#11006,
#11007,#11008,#11009,#11010,#11011,#11012,#11013,#11014,#11015,#11016,#11017,
#11018,#11019,#11020,#11021,#11022,#11023,#11024,#11025,#11026,#11027,#11028,
#11029,#11030,#11031,#11032,#11033,#11034,#11035,#11036,#11037,#11038,#11039,
#11040,#11041,#11042,#11043,#11044,#11045,#11046,#11047,#11048,#11049,#11050,
#11051,#11052,#11053,#11054,#11055,#11056,#11057,#11058,#11059,#11060,#11061,
#11062,#11063,#11064,#11065,#11066,#11067,#11068,#11069,#11070,#11071,#11072,
#11073,#11074,#11075,#11076,#11077,#11078,#11079,#11080,#11081,#11082,#11083,
#11084,#11085,#11086,#11087,#11088,#11089,#11090,#11091,#11092,#11093,#11094,
#11095,#11096,#11097,#11098,#11099,#11100,#11101,#11102,#11103,#11104,#11105,
#11106,#11107,#11108,#11109,#11110,#11111,#11112,#11113,#11114,#11115,#11116,
#11117,#11118,#11119,#11120,#11121,#11122,#11123,#11124,#11125,#11126,#11127,
#11128,#11129,#11130,#11131,#11132,#11133,#11134,#11135,#11136,#11137,#11138,
#11139,#11140,#11141,#11142,#11143,#11144,#11145,#11146,#11147,#11148,#11149,
#11150,#11151,#11152,#11153,#11154,#11155,#11156,#11157,#11158,#11159,#11160,
#11161,#11162,#11163,#11164,#11165,#11166,#11167,#11168,#11169,#11170,#11171,
#11172,#11173,#11174,#11175,#11176,#11177,#11178,#11179,#11180,#11181,#11182,
#11183,#11184,#11185,#11186,#11187,#11188,#11189,#11190,#11191),
 .UNSPECIFIED.,.F.,.F.,(4,2,2,2,2,2,2,2,2,2,2,2,2,2,2,2,2,2,2,2,2,2,2,2,
2,2,2,2,2,2,2,2,2,2,2,2,2,2,2,2,2,2,2,2,2,2,2,2,2,2,2,2,2,2,2,2,2,2,2,2,
2,2,2,2,2,2,2,2,2,2,2,2,2,2,2,2,2,2,2,2,2,2,2,2,2,2,2,2,2,2,2,2,2,2,2,2,
2,2,2,2,2,2,2,2,2,4),(-2.51288241066526,-2.51214445501738,-2.51060224277513,
-2.50790860514932,-2.50338599726915,-2.48645030077016,-2.47441910954673,
-2.4511797341194,-2.42762592101787,-2.42022974928811,-2.41520667626236,
-2.41322566847082,-2.41183598549087,-2.41054988648136,-2.40874200974333,
-2.40391420421472,-2.36807159047678,-2.3365886990444,-2.32022151203857,
-2.31582987750348,-2.31355025120258,-2.31119011739592,-2.30837016025852,
-2.30329613694199,-2.27790866130605,-2.23311754113698,-2.21787546095408,
-2.21499427581866,-2.21340950025191,-2.21205547480733,-2.21032090648445,
-2.2075214636637,-2.19071717656399,-2.14186829819052,-2.12162929848748,
-2.11694550551634,-2.11420553445069,-2.11179032075548,-2.10876986948682,
-2.10406156036042,-2.07723599856565,-2.03798477346606,-2.01900485895288,
-2.01597010135829,-2.0143525348357,-2.01300116913392,-2.01130862524779,
-2.00801792037228,-1.97906797508171,-1.94050984249165,-1.92225585577146,
-1.91771200074851,-1.91500263889804,-1.91258263059342,-1.90951331613283,
-1.90464369616122,-1.86551689275737,-1.83750193776643,-1.8198103364135,
-1.81682260298471,-1.81521500539607,-1.81386302868469,-1.81215840570422,
-1.80945831582091,-1.79473446639502,-1.74393068086411,-1.72340855703997,
-1.71870634799361,-1.71596238252787,-1.71354773036474,-1.71053335828633,
-1.70584493530853,-1.67965802593662,-1.63561252066912,-1.62046884238219,
-1.61759248289826,-1.61600875369154,-1.61465461915812,-1.612918616231,-1.61011436681868,
-1.59319163864348,-1.54445216217191,-1.52422993928622,-1.5195472697316,
-1.51680755321848,-1.51439232056878,-1.51137152418374,-1.50666205293365,
-1.47980224716878,-1.44058212678616,-1.42160779289788,-1.41857323996224,
-1.4169557219418,-1.41560436139287,-1.41391177951697,-1.41062087268735,
-1.38338746555306,-1.34839031277509,-1.33321132179092,-1.32313989675661,
-1.31944004273002,-1.31691299832961,-1.31444319405084,-1.31090563945398,
-1.30439157194774,-1.2568423001509),.UNSPECIFIED.);
#99=B_SPLINE_CURVE_WITH_KNOTS('',3,(#11196,#11197,#11198,#11199,#11200,
#11201,#11202,#11203,#11204,#11205,#11206,#11207,#11208,#11209,#11210,#11211,
#11212,#11213,#11214,#11215,#11216,#11217,#11218,#11219,#11220,#11221,#11222,
#11223,#11224,#11225,#11226,#11227,#11228,#11229,#11230,#11231,#11232,#11233,
#11234,#11235,#11236,#11237,#11238,#11239,#11240,#11241,#11242,#11243,#11244,
#11245,#11246,#11247,#11248,#11249,#11250,#11251,#11252,#11253,#11254,#11255,
#11256,#11257,#11258,#11259,#11260,#11261,#11262,#11263,#11264,#11265,#11266,
#11267,#11268,#11269,#11270,#11271,#11272,#11273,#11274,#11275,#11276,#11277,
#11278,#11279,#11280,#11281,#11282,#11283,#11284,#11285,#11286,#11287,#11288,
#11289,#11290,#11291,#11292,#11293,#11294,#11295,#11296,#11297,#11298,#11299,
#11300,#11301,#11302,#11303,#11304,#11305,#11306,#11307,#11308,#11309,#11310,
#11311,#11312,#11313,#11314,#11315,#11316,#11317,#11318,#11319,#11320,#11321,
#11322,#11323,#11324,#11325,#11326,#11327,#11328,#11329,#11330,#11331,#11332,
#11333,#11334,#11335,#11336,#11337,#11338,#11339,#11340,#11341,#11342,#11343,
#11344,#11345,#11346,#11347,#11348,#11349,#11350,#11351,#11352,#11353,#11354,
#11355,#11356,#11357,#11358,#11359,#11360,#11361,#11362,#11363,#11364,#11365,
#11366,#11367,#11368,#11369,#11370,#11371,#11372,#11373,#11374,#11375,#11376,
#11377,#11378,#11379,#11380,#11381,#11382,#11383,#11384,#11385,#11386,#11387,
#11388,#11389,#11390,#11391,#11392,#11393,#11394,#11395,#11396,#11397,#11398,
#11399,#11400,#11401,#11402,#11403),.UNSPECIFIED.,.F.,.F.,(4,2,2,2,2,2,
2,2,2,2,2,2,2,2,2,2,2,2,2,2,2,2,2,2,2,2,2,2,2,2,2,2,2,2,2,2,2,2,2,2,2,2,
2,2,2,2,2,2,2,2,2,2,2,2,2,2,2,2,2,2,2,2,2,2,2,2,2,2,2,2,2,2,2,2,2,2,2,2,
2,2,2,2,2,2,2,2,2,2,2,2,2,2,2,2,2,2,2,2,2,2,2,2,2,4),(-1.2571395732103,
-1.21587274758227,-1.17959905046059,-1.17478545014533,-1.17297907343572,
-1.17169312534346,-1.17030256268692,-1.16831859623973,-1.16327894066679,
-1.1558518451504,-1.13213488728549,-1.08438557842686,-1.07787401689846,
-1.07433668667642,-1.07186649978398,-1.06933861031397,-1.06563668276486,
-1.05555442071088,-1.04035235318455,-1.00516879234281,-0.978093046261673,
-0.974801173174284,-0.973108132803348,-0.971756426298004,-0.970138511402003,
-0.967103275275226,-0.94812300442694,-0.908847135917745,-0.882063884310117,
-0.877356297404026,-0.874335625987243,-0.87191981433345,-0.869178711195009,
-0.864491858203241,-0.844221568498299,-0.795208829567818,-0.77852885281364,
-0.77573382360805,-0.774000321739977,-0.772646025083837,-0.77105963539429,
-0.768172298874631,-0.752814518413845,-0.707121594213327,-0.682686981858239,
-0.678069153500248,-0.675075799817945,-0.672662133857943,-0.669902026562685,
-0.665128364851073,-0.643477856951114,-0.595049789996574,-0.579250061705756,
-0.576493366971042,-0.574771355188765,-0.573417875569529,-0.571822888318959,
-0.568895703176516,-0.552678219397519,-0.498884531695963,-0.482450998923153,
-0.477874069639845,-0.47515699661495,-0.472979522737904,-0.470038419377697,
-0.464413199315306,-0.422615631294253,-0.382569438506089,-0.377922750983697,
-0.376138368740135,-0.374858215763686,-0.373462655829577,-0.371452885587081,
-0.366246055918608,-0.35848866151363,-0.332921653310087,-0.287847258389022,
-0.280436456141002,-0.277481670090351,-0.27501825796628,-0.27248141749682,
-0.268736610879544,-0.258344077884017,-0.242496420805238,-0.215202655607788,
-0.183744354591778,-0.178839674545282,-0.176820143031453,-0.175436584436919,
-0.174016157870222,-0.171906553255985,-0.169369999632317,-0.164563042519488,
-0.152552126040816,-0.127153744163367,-0.0890005180998729,-0.0815382465895854,
-0.0784945098849429,-0.0762338182520622,-0.0737598403893136,-0.0703355435282101,
-0.0620912127834048,-0.0504812419885443,-0.000709656257275801),
 .UNSPECIFIED.);
#100=B_SPLINE_CURVE_WITH_KNOTS('',3,(#11404,#11405,#11406,#11407,#11408,
#11409,#11410,#11411,#11412,#11413,#11414,#11415,#11416,#11417,#11418,#11419,
#11420,#11421,#11422,#11423,#11424,#11425,#11426,#11427,#11428,#11429,#11430,
#11431,#11432,#11433,#11434,#11435,#11436,#11437,#11438,#11439,#11440,#11441,
#11442,#11443,#11444,#11445,#11446,#11447,#11448,#11449,#11450,#11451,#11452,
#11453,#11454,#11455,#11456,#11457,#11458,#11459,#11460,#11461,#11462,#11463,
#11464,#11465,#11466,#11467,#11468,#11469,#11470,#11471,#11472,#11473,#11474,
#11475,#11476,#11477,#11478,#11479,#11480,#11481,#11482,#11483,#11484,#11485,
#11486,#11487,#11488,#11489,#11490,#11491,#11492,#11493,#11494,#11495,#11496,
#11497,#11498,#11499,#11500,#11501,#11502,#11503,#11504,#11505,#11506,#11507,
#11508,#11509,#11510,#11511,#11512,#11513,#11514,#11515,#11516,#11517,#11518,
#11519,#11520,#11521,#11522,#11523,#11524,#11525,#11526,#11527,#11528,#11529,
#11530,#11531,#11532,#11533,#11534,#11535,#11536,#11537,#11538,#11539,#11540,
#11541,#11542,#11543,#11544,#11545,#11546,#11547,#11548,#11549,#11550,#11551,
#11552,#11553,#11554,#11555,#11556,#11557,#11558,#11559,#11560,#11561,#11562,
#11563,#11564,#11565,#11566,#11567,#11568,#11569,#11570,#11571,#11572,#11573,
#11574,#11575,#11576,#11577,#11578,#11579,#11580,#11581,#11582,#11583,#11584,
#11585,#11586,#11587,#11588,#11589,#11590,#11591,#11592,#11593,#11594,#11595,
#11596,#11597,#11598,#11599,#11600,#11601,#11602,#11603,#11604,#11605,#11606,
#11607,#11608,#11609,#11610,#11611,#11612,#11613,#11614,#11615,#11616,#11617,
#11618,#11619,#11620,#11621,#11622,#11623,#11624,#11625,#11626,#11627,#11628,
#11629,#11630,#11631,#11632,#11633,#11634,#11635,#11636,#11637,#11638,#11639,
#11640,#11641,#11642,#11643,#11644,#11645,#11646,#11647,#11648,#11649,#11650,
#11651,#11652,#11653,#11654,#11655,#11656,#11657,#11658,#11659,#11660,#11661,
#11662,#11663,#11664,#11665,#11666,#11667,#11668,#11669,#11670,#11671,#11672,
#11673,#11674,#11675),.UNSPECIFIED.,.F.,.F.,(4,2,2,2,2,2,2,2,2,2,2,2,2,
2,2,2,2,2,2,2,2,2,2,2,2,2,2,2,2,2,2,2,2,2,2,2,2,2,2,2,2,2,2,2,2,2,2,2,2,
2,2,2,2,2,2,2,2,2,2,2,2,2,2,2,2,2,2,2,2,2,2,2,2,2,2,2,2,2,2,2,2,2,2,2,2,
2,2,2,2,2,2,2,2,2,2,2,2,2,2,2,2,2,2,2,2,2,2,2,2,2,2,2,2,2,2,2,2,2,2,2,2,
2,2,2,2,2,2,2,2,2,2,2,2,2,2,4),(-1.2568423001509,-1.2566698222456,-1.22541220817351,
-1.22051497282777,-1.21849696950792,-1.21711394976688,-1.21566446046196,
-1.21339786217466,-1.20625643975202,-1.19427227502351,-1.16634924188049,
-1.12726561901582,-1.12239584948917,-1.11932638806809,-1.11690624854978,
-1.11419672336264,-1.10965256110062,-1.09139783300629,-1.05284084188285,
-1.02384290342377,-1.02055154933599,-1.01885879412598,-1.01750732510715,
-1.01588970615908,-1.0128550566056,-0.993879639747066,-0.954619185808075,
-0.927831209380359,-0.923124124737194,-0.920103885873031,-0.91768849096575,
-0.914947936776402,-0.910262212208136,-0.890000098150051,-0.8410263697577,
-0.824316438153823,-0.821520532228975,-0.819786925448196,-0.818432835038808,
-0.81684702213994,-0.813961573251889,-0.798635081334897,-0.753177254540022,
-0.728508971189148,-0.723881885248253,-0.720885979558173,-0.718472503499583,
-0.715715066193194,-0.710952272498883,-0.689471978183512,-0.629594428850235,
-0.62345090106714,-0.621236501208349,-0.619941235062353,-0.618557484133402,
-0.61661059042971,-0.611804736155214,-0.587317023325035,-0.546955962271519,
-0.528573099819053,-0.523885693868055,-0.521117519767615,-0.518704625799575,
-0.515722333832088,-0.50989605779365,-0.468541453264623,-0.428356469632953,
-0.423727618598784,-0.42194576611162,-0.420666259190551,-0.419270060004242,
-0.417257134481112,-0.412029725890219,-0.404231361134605,-0.378427412343682,
-0.33368169747574,-0.326254049827473,-0.323296542279631,-0.320832392678563,
-0.318296365322415,-0.31455571753035,-0.304194204918573,-0.288411841575985,
-0.256781843283623,-0.227066115286565,-0.223790139820875,-0.222100419016791,
-0.220748735840961,-0.220742813218816,-0.220736969505651,-0.220731203506629,
-0.220725514037649,-0.220719899972107,-0.220714360174469,-0.220708893523408,
-0.220703498924682,-0.220698175293754,-0.22069292159715,-0.22068773679388,
-0.220682619843728,-0.220677569763452,-0.220672585565024,-0.220667666277393,
-0.220662810925145,-0.220658018589557,-0.220653288358301,-0.220648619309919,
-0.22064401057169,-0.220639461272971,-0.220634970523,-0.220630537475715,
-0.220626161317182,-0.220621841213998,-0.220617576367928,-0.220613071472846,
-0.218961874607189,-0.215733042849444,-0.211516000878359,-0.167272700134033,
-0.131388197292718,-0.126491494100865,-0.123413513883083,-0.120991920219225,
-0.118286243819702,-0.113761631106796,-0.0957742494569127,-0.0481363768823709,
-0.0369810077054305,-0.0267619536485706,-0.0241129102553496,-0.0225631826468939,
-0.0212349028317719,-0.0199043353833102,-0.0181638798968172,-0.0153923940619404,
-0.000584983237805827),.UNSPECIFIED.);
#101=B_SPLINE_CURVE_WITH_KNOTS('',3,(#11680,#11681,#11682,#11683,#11684,
#11685,#11686,#11687,#11688,#11689,#11690,#11691,#11692,#11693,#11694,#11695,
#11696,#11697,#11698,#11699,#11700,#11701,#11702,#11703,#11704,#11705,#11706,
#11707,#11708,#11709,#11710,#11711,#11712,#11713,#11714,#11715,#11716,#11717,
#11718,#11719,#11720,#11721,#11722,#11723,#11724,#11725,#11726,#11727,#11728,
#11729,#11730,#11731,#11732,#11733,#11734,#11735,#11736,#11737,#11738,#11739,
#11740,#11741,#11742,#11743,#11744,#11745,#11746,#11747,#11748,#11749,#11750,
#11751,#11752,#11753,#11754,#11755,#11756,#11757,#11758,#11759,#11760,#11761,
#11762,#11763,#11764,#11765,#11766,#11767,#11768,#11769,#11770,#11771,#11772,
#11773,#11774,#11775,#11776,#11777,#11778,#11779,#11780,#11781,#11782,#11783,
#11784,#11785,#11786,#11787,#11788,#11789,#11790,#11791,#11792,#11793,#11794,
#11795,#11796,#11797,#11798,#11799,#11800,#11801,#11802,#11803,#11804,#11805,
#11806,#11807,#11808,#11809,#11810,#11811,#11812,#11813,#11814,#11815,#11816,
#11817,#11818,#11819,#11820,#11821,#11822,#11823,#11824,#11825,#11826,#11827,
#11828,#11829,#11830,#11831,#11832,#11833,#11834,#11835,#11836,#11837,#11838,
#11839,#11840,#11841,#11842,#11843,#11844,#11845,#11846,#11847,#11848,#11849,
#11850,#11851,#11852,#11853,#11854,#11855,#11856,#11857,#11858,#11859,#11860,
#11861,#11862,#11863,#11864,#11865,#11866,#11867,#11868,#11869,#11870,#11871,
#11872,#11873,#11874,#11875,#11876,#11877,#11878,#11879,#11880,#11881,#11882,
#11883,#11884,#11885,#11886,#11887,#11888,#11889,#11890,#11891,#11892,#11893,
#11894,#11895,#11896,#11897,#11898,#11899,#11900,#11901,#11902,#11903,#11904,
#11905),.UNSPECIFIED.,.F.,.F.,(4,2,2,2,2,2,2,2,2,2,2,2,2,2,2,2,2,2,2,2,
2,2,2,2,2,2,2,2,2,2,2,2,2,2,2,2,2,2,2,2,2,2,2,2,2,2,2,2,2,2,2,2,2,2,2,2,
2,2,2,2,2,2,2,2,2,2,2,2,2,2,2,2,2,2,2,2,2,2,2,2,2,2,2,2,2,2,2,2,2,2,2,2,
2,2,2,2,2,2,2,2,2,2,2,2,2,2,2,2,2,2,2,2,4),(-2.5135518234981,-2.47659661189999,
-2.47236394980857,-2.46954258796683,-2.4668230303502,-2.46440446366006,
-2.46135122278182,-2.45653542941664,-2.42634523323622,-2.40243503862959,
-2.37764166219088,-2.37034208190646,-2.36862191645876,-2.36701353481963,
-2.36566149194363,-2.36395753638232,-2.36125988735885,-2.34658797162409,
-2.34299810396128,-2.33833144470471,-2.2994607991541,-2.2836681912839,-2.27670083268194,
-2.27122335335112,-2.26828169159173,-2.26587165891324,-2.26307310110431,
-2.25825131703111,-2.23802946477239,-2.19153911663431,-2.17255181116262,
-2.16951642227373,-2.16789856775074,-2.16654698975295,-2.16485421556432,
-2.16156316551322,-2.13290948589647,-2.09410750441372,-2.0757949541683,
-2.07124618961755,-2.06853548053722,-2.06611525428305,-2.06304700262955,
-2.05818175003555,-2.0185046895441,-1.98833052162263,-1.97313430702212,
-1.97025501678423,-1.96867049511841,-1.96731619519208,-1.96558064117932,
-1.96277838846072,-1.94591371543415,-1.89711011504228,-1.87687596239538,
-1.87219194986349,-1.86945165473324,-1.86703603717352,-1.86401492471449,
-1.85930528178858,-1.83245871193674,-1.79321616035522,-1.77423584936763,
-1.77120069502457,-1.769582887682,-1.76823130366523,-1.76653846484517,-1.76324712459706,
-1.73420957683203,-1.69571076542024,-1.67746927051293,-1.67292584867029,
-1.67021630620254,-1.66779586259606,-1.66472562338087,-1.65985378951481,
-1.62075026642361,-1.5928054348406,-1.5750158236052,-1.57202393976116,-1.57041530281815,
-1.56906316168771,-1.56735922955389,-1.56466188885155,-1.5499991950463,
-1.54641876152499,-1.5330158196089,-1.50294444773783,-1.48710576600214,
-1.47671678354855,-1.4729727360809,-1.4704362484655,-1.46797305379231,-1.46501836655225,
-1.45760704584601,-1.41257226268484,-1.38694949731365,-1.37918258791311,
-1.37397155702751,-1.37196127208251,-1.3705657223838,-1.3692858663284,-1.36750229257816,
-1.3628602896076,-1.32309258642019,-1.29427990913698,-1.28399829066645,
-1.27648602457344,-1.2731857217843,-1.27073334466664,-1.26844402289056,
-1.26528627603858,-1.2571395732103),.UNSPECIFIED.);
#102=B_SPLINE_CURVE_WITH_KNOTS('',3,(#11906,#11907,#11908,#11909,#11910,
#11911,#11912,#11913,#11914,#11915),.UNSPECIFIED.,.F.,.F.,(4,1,1,1,1,1,
1,4),(97.3893809475092,98.2770128807329,99.2731119575535,100.269211034374,
101.265310111195,102.261409188015,103.257508264836,103.672551685613),
 .UNSPECIFIED.);
#103=B_SPLINE_CURVE_WITH_KNOTS('',3,(#11920,#11921,#11922,#11923,#11924,
#11925,#11926,#11927,#11928,#11929,#11930),.UNSPECIFIED.,.F.,.F.,(4,1,1,
1,1,1,1,1,4),(103.672560201549,103.933669101939,104.92976817876,105.925867255581,
106.921966332401,107.918065409222,108.914164486042,109.910263562863,109.955742875643),
 .UNSPECIFIED.);
#104=B_SPLINE_CURVE_WITH_KNOTS('',3,(#11931,#11932,#11933,#11934,#11935,
#11936,#11937,#11938,#11939,#11940,#11941,#11942,#11943,#11944,#11945,#11946,
#11947,#11948,#11949,#11950,#11951,#11952,#11953,#11954,#11955,#11956,#11957,
#11958,#11959,#11960,#11961,#11962,#11963,#11964,#11965,#11966,#11967,#11968,
#11969,#11970,#11971,#11972,#11973,#11974,#11975,#11976,#11977,#11978,#11979,
#11980,#11981,#11982,#11983,#11984,#11985,#11986,#11987,#11988,#11989,#11990,
#11991,#11992,#11993,#11994,#11995,#11996,#11997,#11998,#11999,#12000,#12001,
#12002,#12003,#12004,#12005,#12006,#12007,#12008,#12009,#12010,#12011,#12012,
#12013,#12014,#12015,#12016,#12017,#12018,#12019,#12020,#12021,#12022,#12023,
#12024,#12025,#12026,#12027,#12028,#12029,#12030,#12031,#12032,#12033,#12034,
#12035,#12036,#12037,#12038,#12039,#12040,#12041,#12042,#12043,#12044,#12045,
#12046,#12047,#12048,#12049,#12050,#12051,#12052,#12053,#12054,#12055,#12056,
#12057,#12058,#12059,#12060,#12061,#12062,#12063,#12064,#12065,#12066,#12067,
#12068,#12069,#12070,#12071,#12072,#12073,#12074,#12075,#12076,#12077,#12078,
#12079,#12080,#12081,#12082,#12083,#12084,#12085,#12086,#12087,#12088,#12089,
#12090,#12091,#12092,#12093,#12094,#12095,#12096,#12097,#12098,#12099,#12100,
#12101,#12102,#12103,#12104,#12105,#12106,#12107,#12108,#12109,#12110,#12111,
#12112,#12113,#12114,#12115,#12116,#12117,#12118,#12119,#12120,#12121,#12122,
#12123,#12124,#12125,#12126,#12127,#12128,#12129,#12130,#12131,#12132,#12133,
#12134,#12135,#12136,#12137,#12138,#12139,#12140,#12141,#12142,#12143,#12144,
#12145,#12146,#12147,#12148),.UNSPECIFIED.,.F.,.F.,(4,2,2,2,2,2,2,2,2,2,
2,2,2,2,2,2,2,2,2,2,2,2,2,2,2,2,2,2,2,2,2,2,2,2,2,2,2,2,2,2,2,2,2,2,2,2,
2,2,2,2,2,2,2,2,2,2,2,2,2,2,2,2,2,2,2,2,2,2,2,2,2,2,2,2,2,2,2,2,2,2,2,2,
2,2,2,2,2,2,2,2,2,2,2,2,2,2,2,2,2,2,2,2,2,2,2,2,2,2,4),(-2.51313020307964,
-2.50351913808445,-2.50050660773422,-2.49815843919155,-2.49581373346396,
-2.49314272965445,-2.48877172810962,-2.47435014552162,-2.42228289418547,
-2.40219469446745,-2.39912406872919,-2.39749907227943,-2.3961482485783,
-2.39446481911957,-2.3912158846612,-2.36793986594067,-2.33408335644315,
-2.31567916766454,-2.30795000318622,-2.30372337978279,-2.30090475510632,
-2.29823464985763,-2.29584041929594,-2.29282152493645,-2.2881178180231,
-2.26151404940473,-2.22207530174103,-2.20306331629715,-2.20002769171616,
-2.19841003763219,-2.19705881734433,-2.19536673018494,-2.19207770441167,
-2.16537599340211,-2.13034325459464,-2.11486423377487,-2.10799250833549,
-2.1025149943886,-2.0996051560735,-2.09721954594407,-2.09440390519471,-2.0895056516581,
-2.06811523218513,-2.02397008969713,-2.00402221278937,-2.00095571201658,
-1.99933148154723,-1.99798047831947,-1.99629580463093,-1.99304157252599,
-1.96943828362305,-1.94082968756209,-1.91141036606866,-1.90433587884971,
-1.90111409058145,-1.89867444862865,-1.89636343395275,-1.8924691711515,
-1.88188348039685,-1.82137096305922,-1.80465191282259,-1.80170330066452,
-1.80010392014619,-1.79875112235557,-1.79703561297581,-1.7942999233654,
-1.77884704784025,-1.76194506009828,-1.76085454667944,-1.72582171983243,
-1.71404391167468,-1.70570869505985,-1.7022698871658,-1.69979352346803,
-1.69753617017616,-1.69393167030004,-1.68716690334331,-1.64438646555818,
-1.60948306158413,-1.60382417254802,-1.60174805580431,-1.60033934262863,
-1.59907256916522,-1.59700637548609,-1.59182127597304,-1.53134688725329,
-1.50928203603504,-1.50448466034263,-1.50171971246554,-1.4993070443035,
-1.49632169307475,-1.49172901778547,-1.46787020047601,-1.42593250836169,
-1.40646244030087,-1.40341089885887,-1.40178966175489,-1.40043829387519,
-1.39874958850897,-1.39547736270904,-1.36549513075084,-1.32771629500846,
-1.30964708016495,-1.30511684989029,-1.30241025822242,-1.29998937402529,
-1.29691438225343,-1.29202658440206,-1.25692875797613),.UNSPECIFIED.);
#105=B_SPLINE_CURVE_WITH_KNOTS('',3,(#12153,#12154,#12155,#12156,#12157,
#12158,#12159,#12160,#12161,#12162,#12163,#12164,#12165,#12166,#12167,#12168,
#12169,#12170,#12171,#12172,#12173,#12174,#12175,#12176,#12177,#12178,#12179,
#12180,#12181,#12182,#12183,#12184,#12185,#12186,#12187,#12188,#12189,#12190,
#12191,#12192,#12193,#12194,#12195,#12196,#12197,#12198,#12199,#12200,#12201,
#12202,#12203,#12204,#12205,#12206,#12207,#12208,#12209,#12210,#12211,#12212,
#12213,#12214,#12215,#12216,#12217,#12218,#12219,#12220,#12221,#12222,#12223,
#12224,#12225,#12226,#12227,#12228,#12229,#12230,#12231,#12232,#12233,#12234,
#12235,#12236,#12237,#12238,#12239,#12240,#12241,#12242,#12243,#12244,#12245,
#12246,#12247,#12248,#12249,#12250,#12251,#12252,#12253,#12254,#12255,#12256,
#12257,#12258,#12259,#12260,#12261,#12262,#12263,#12264,#12265,#12266,#12267,
#12268,#12269,#12270,#12271,#12272,#12273,#12274,#12275,#12276,#12277,#12278,
#12279,#12280,#12281,#12282,#12283,#12284,#12285,#12286,#12287,#12288,#12289,
#12290,#12291,#12292,#12293,#12294,#12295,#12296,#12297,#12298,#12299,#12300,
#12301,#12302,#12303,#12304,#12305,#12306,#12307,#12308,#12309,#12310,#12311,
#12312,#12313,#12314,#12315,#12316,#12317,#12318,#12319,#12320,#12321,#12322,
#12323,#12324,#12325,#12326,#12327,#12328,#12329,#12330,#12331,#12332,#12333,
#12334,#12335,#12336,#12337,#12338,#12339),.UNSPECIFIED.,.F.,.F.,(4,3,3,
3,3,3,3,3,3,3,3,3,3,3,3,3,3,3,3,3,3,3,3,3,3,3,3,3,3,3,3,3,3,3,3,3,3,3,3,
3,3,3,3,3,3,3,3,3,3,3,3,3,3,3,3,3,3,3,3,3,3,3,4),(109.955743251696,110.0599685937,
110.165767849448,110.269723962552,110.37362116787,110.477496011397,110.584712668469,
110.688717274338,110.79753995701,110.906362639683,111.011342877977,111.116166140091,
111.22086671262,111.325501816955,111.430106980845,111.534717688392,111.639438820454,
111.744221384281,111.849184855582,111.902461716504,112.007441954798,112.112265216913,
112.216965789442,112.321600893777,112.426206057666,112.530816765213,112.635537897276,
112.740320461102,112.845283932403,112.898560793325,113.003541031619,113.108364293734,
113.213064866263,113.317699970598,113.422305134487,113.526915842034,113.631636974096,
113.736419537923,113.841383009224,113.894659870145,113.999640108439,114.104463370553,
114.209163943082,114.313799047417,114.418404211306,114.523014918853,114.627736050915,
114.732518614742,114.837482086043,114.890758946966,114.99573918526,115.100562447374,
115.205263019903,115.309898124238,115.414503288127,115.519113995675,115.623835127737,
115.728617691563,115.833581162864,115.886858023786,116.007775537452,116.127668495559,
116.238928182439),.UNSPECIFIED.);
#106=B_SPLINE_CURVE_WITH_KNOTS('',3,(#12340,#12341,#12342,#12343,#12344,
#12345,#12346,#12347,#12348,#12349,#12350,#12351,#12352,#12353,#12354,#12355,
#12356,#12357,#12358,#12359,#12360,#12361,#12362,#12363,#12364,#12365,#12366,
#12367,#12368,#12369,#12370,#12371,#12372,#12373,#12374,#12375,#12376,#12377,
#12378,#12379,#12380,#12381,#12382,#12383,#12384,#12385,#12386,#12387,#12388,
#12389,#12390,#12391,#12392,#12393,#12394,#12395,#12396,#12397,#12398,#12399,
#12400,#12401,#12402,#12403,#12404,#12405,#12406,#12407,#12408,#12409,#12410,
#12411,#12412,#12413,#12414,#12415,#12416,#12417,#12418,#12419,#12420,#12421,
#12422,#12423,#12424,#12425,#12426,#12427,#12428,#12429,#12430,#12431,#12432,
#12433,#12434,#12435,#12436,#12437,#12438,#12439,#12440,#12441,#12442,#12443,
#12444,#12445,#12446,#12447,#12448,#12449,#12450,#12451,#12452,#12453,#12454,
#12455,#12456,#12457,#12458,#12459,#12460,#12461,#12462,#12463,#12464,#12465,
#12466,#12467,#12468,#12469,#12470,#12471,#12472,#12473,#12474,#12475,#12476,
#12477,#12478,#12479,#12480,#12481,#12482,#12483,#12484,#12485,#12486,#12487,
#12488,#12489,#12490,#12491,#12492,#12493,#12494,#12495,#12496,#12497,#12498,
#12499,#12500,#12501,#12502,#12503,#12504,#12505,#12506,#12507,#12508,#12509,
#12510,#12511,#12512,#12513,#12514,#12515,#12516,#12517,#12518,#12519,#12520,
#12521,#12522,#12523,#12524,#12525,#12526,#12527,#12528,#12529,#12530,#12531,
#12532,#12533,#12534,#12535,#12536,#12537,#12538,#12539,#12540,#12541,#12542,
#12543,#12544,#12545,#12546,#12547,#12548,#12549,#12550,#12551,#12552,#12553,
#12554,#12555,#12556,#12557,#12558,#12559),.UNSPECIFIED.,.F.,.F.,(4,2,2,
2,2,2,2,2,2,2,2,2,2,2,2,2,2,2,2,2,2,2,2,2,2,2,2,2,2,2,2,2,2,2,2,2,2,2,2,
2,2,2,2,2,2,2,2,2,2,2,2,2,2,2,2,2,2,2,2,2,2,2,2,2,2,2,2,2,2,2,2,2,2,2,2,
2,2,2,2,2,2,2,2,2,2,2,2,2,2,2,2,2,2,2,2,2,2,2,2,2,2,2,2,2,2,2,2,2,2,4),
(-1.25692875797613,-1.25674831771628,-1.22109814401454,-1.20715075077619,
-1.20449051608729,-1.20279788698641,-1.20144633454568,-1.1998283961176,
-1.1967925573605,-1.17778734641612,-1.13836384625689,-1.11175241982937,
-1.10705117788052,-1.10403260656388,-1.10161720746712,-1.09887520972168,
-1.09418342389249,-1.07383245908521,-1.02426810723142,-1.00818857747104,
-1.00541920541137,-1.00369349892358,-1.00233992095459,-1.00074809730998,
-0.997835044481727,-0.981924555709882,-0.931350460638727,-0.911852785541992,
-0.907083010806373,-0.904296230703167,-0.901885275858441,-0.898928499815264,
-0.893226073892296,-0.855647249789531,-0.814535503365626,-0.807618670692958,
-0.805298804606913,-0.803982731547137,-0.802611038654916,-0.800735047090535,
-0.796353602195302,-0.776073782845448,-0.724783548047366,-0.711541064934163,
-0.707300771921169,-0.704657775026998,-0.702221051071134,-0.699021700695893,
-0.692071862773937,-0.663679770802434,-0.628974429634597,-0.62415353701392,
-0.609670369508724,-0.6069820543422,-0.605280876782828,-0.603928896096546,
-0.602318038585365,-0.59931567660915,-0.581245868062967,-0.553504271993497,
-0.514543897039331,-0.509670307516983,-0.506599531012716,-0.504179036587773,
-0.501469825824454,-0.496927898468081,-0.478707058558699,-0.440297590914658,
-0.411082827878853,-0.40780432224785,-0.406114220230819,-0.404762732065709,
-0.403142536400415,-0.400096172631472,-0.380782076248408,-0.33964293640904,
-0.314929269570648,-0.31030005382914,-0.307303398667504,-0.304889728850224,
-0.302132517267191,-0.297371251381643,-0.275919695926451,-0.216442002964044,
-0.209960938661077,-0.20769961356291,-0.206395046823953,-0.205044563880018,
-0.203190572090568,-0.201086698355723,-0.197412573419394,-0.189274121239726,
-0.161425992263691,-0.119455369380977,-0.112076068539679,-0.109046552799285,
-0.106789281207341,-0.104312033687726,-0.10087020412236,-0.0925187169600056,
-0.0807098673079125,-0.0392913683885479,-0.0182779886034172,-0.010989094082505,
-0.00862216523462031,-0.00715023010479006,-0.00586260496413733,-0.00449433525428351,
-0.00256109856699574,-0.000585265855186645),.UNSPECIFIED.);
#107=B_SPLINE_CURVE_WITH_KNOTS('',3,(#12564,#12565,#12566,#12567,#12568,
#12569,#12570,#12571,#12572,#12573,#12574,#12575,#12576,#12577,#12578,#12579,
#12580,#12581,#12582,#12583,#12584,#12585,#12586,#12587,#12588,#12589,#12590,
#12591,#12592,#12593,#12594,#12595,#12596,#12597,#12598,#12599,#12600,#12601,
#12602,#12603,#12604,#12605,#12606,#12607,#12608,#12609,#12610,#12611,#12612,
#12613,#12614,#12615,#12616,#12617,#12618,#12619,#12620,#12621,#12622,#12623,
#12624,#12625,#12626,#12627,#12628,#12629,#12630,#12631,#12632,#12633,#12634,
#12635,#12636,#12637,#12638,#12639,#12640,#12641,#12642,#12643,#12644,#12645,
#12646,#12647,#12648,#12649,#12650,#12651,#12652,#12653,#12654,#12655,#12656,
#12657,#12658,#12659,#12660,#12661,#12662,#12663,#12664,#12665,#12666,#12667,
#12668,#12669,#12670,#12671,#12672,#12673,#12674,#12675,#12676,#12677,#12678,
#12679,#12680,#12681,#12682,#12683,#12684,#12685,#12686,#12687,#12688,#12689,
#12690,#12691,#12692,#12693,#12694,#12695,#12696,#12697,#12698,#12699,#12700,
#12701,#12702,#12703,#12704,#12705,#12706,#12707,#12708,#12709,#12710,#12711,
#12712,#12713,#12714,#12715,#12716,#12717,#12718,#12719,#12720,#12721,#12722,
#12723,#12724,#12725,#12726,#12727,#12728,#12729,#12730,#12731,#12732,#12733,
#12734,#12735,#12736,#12737,#12738,#12739,#12740,#12741,#12742,#12743,#12744,
#12745,#12746,#12747,#12748,#12749,#12750,#12751,#12752,#12753,#12754,#12755,
#12756,#12757,#12758,#12759,#12760,#12761,#12762,#12763,#12764,#12765,#12766,
#12767,#12768,#12769,#12770,#12771,#12772,#12773,#12774,#12775,#12776,#12777,
#12778,#12779,#12780,#12781,#12782,#12783,#12784,#12785,#12786,#12787,#12788,
#12789,#12790,#12791,#12792,#12793,#12794,#12795,#12796,#12797,#12798,#12799,
#12800,#12801,#12802,#12803,#12804,#12805,#12806,#12807,#12808,#12809,#12810,
#12811,#12812,#12813,#12814,#12815,#12816,#12817),.UNSPECIFIED.,.F.,.F.,
(4,2,2,2,2,2,2,2,2,2,2,2,2,2,2,2,2,2,2,2,2,2,2,2,2,2,2,2,2,2,2,2,2,2,2,
2,2,2,2,2,2,2,2,2,2,2,2,2,2,2,2,2,2,2,2,2,2,2,2,2,2,2,2,2,2,2,2,2,2,2,2,
2,2,2,2,2,2,2,2,2,2,2,2,2,2,2,2,2,2,2,2,2,2,2,2,2,2,2,2,2,2,2,2,2,2,2,2,
2,2,2,2,2,2,2,2,2,2,2,2,2,2,2,2,2,2,2,4),(-1.25721314605092,-1.23410841050774,
-1.22954161186543,-1.22656375576533,-1.22415102282358,-1.2213792528173,
-1.21655262850479,-1.1939961644514,-1.16352389726284,-1.14680516878331,
-1.13082265003821,-1.12805720747367,-1.1263325710184,-1.12497891679185,
-1.12338593268706,-1.12046804004912,-1.10445722586107,-1.05289135589093,
-1.03435531751347,-1.02965198137857,-1.02688019427728,-1.02446769410289,
-1.0214904436709,-1.01568879368394,-0.975133357582088,-0.934045095177474,
-0.929463525901543,-0.927688776187349,-0.926411150294908,-0.925013288919188,
-0.922991762752392,-0.917707210838215,-0.90979442286352,-0.883317223127766,
-0.839502033391039,-0.83203204238506,-0.82906786170256,-0.826602039218295,
-0.824068271270609,-0.820338421416605,-0.810055608898703,-0.794437841170515,
-0.760313609126218,-0.732852138489897,-0.72955954685681,-0.727866277201391,
-0.726514463180541,-0.72489650969611,-0.721861443067769,-0.702891381175583,
-0.663678137920787,-0.636819808664008,-0.632109334575591,-0.629087663546109,
-0.62667160003942,-0.623930799418827,-0.619245930790415,-0.599009663918522,
-0.550226702083068,-0.533292055105846,-0.530486400260093,-0.528749647696569,
-0.527394999157189,-0.525810737980295,-0.522933607471545,-0.507788863622081,
-0.463746243340883,-0.437564045080649,-0.43287495247255,-0.429859726370079,
-0.42744413412075,-0.424698824012465,-0.419993625127158,-0.399447804412861,
-0.348533978060796,-0.333863207189271,-0.331164830994524,-0.329460351564713,
-0.328107839038345,-0.326498826255675,-0.323506434495639,-0.305716982370102,
-0.277771298222007,-0.23869810383822,-0.233819850544559,-0.230747217691625,
-0.228325935105404,-0.228286333013025,-0.228232330027664,-0.228182580458323,
-0.228136740536762,-0.228094494714532,-0.22805555347062,-0.228019651229689,
-0.227986544399185,-0.227956009547196,-0.227927841703126,-0.227901852799441,
-0.227877870239158,-0.227855735569204,-0.22783530328297,-0.227816439721745,
-0.227787725550702,-0.227759502646055,-0.22773175972712,-0.224849511854618,
-0.219429371895256,-0.212575646028398,-0.197158165912927,-0.161712336597581,
-0.135229983426135,-0.131940067678489,-0.130247256307972,-0.128895313480881,
-0.127276615593005,-0.124238566824772,-0.105189659513025,-0.0640561891760269,
-0.0479072815185143,-0.03680636699023,-0.0328382146543954,-0.0305122524671761,
-0.0281761769943295,-0.0258175261057142,-0.0227753831788527,-0.0147912398161514,
-0.000585061531517047),.UNSPECIFIED.);
#108=B_SPLINE_CURVE_WITH_KNOTS('',3,(#12818,#12819,#12820,#12821,#12822,
#12823,#12824,#12825,#12826,#12827,#12828,#12829,#12830,#12831,#12832,#12833,
#12834,#12835,#12836,#12837,#12838,#12839,#12840,#12841,#12842,#12843,#12844,
#12845,#12846,#12847,#12848,#12849,#12850,#12851,#12852,#12853,#12854,#12855,
#12856,#12857,#12858,#12859,#12860,#12861,#12862,#12863,#12864,#12865,#12866,
#12867,#12868,#12869,#12870,#12871,#12872,#12873,#12874,#12875,#12876,#12877,
#12878,#12879,#12880,#12881,#12882,#12883,#12884,#12885,#12886,#12887,#12888,
#12889,#12890,#12891,#12892,#12893,#12894,#12895,#12896,#12897,#12898,#12899,
#12900,#12901,#12902,#12903,#12904,#12905,#12906,#12907,#12908,#12909,#12910,
#12911,#12912,#12913,#12914,#12915,#12916,#12917,#12918,#12919,#12920,#12921,
#12922,#12923,#12924,#12925,#12926,#12927,#12928,#12929,#12930,#12931,#12932,
#12933,#12934,#12935,#12936,#12937,#12938,#12939,#12940,#12941,#12942,#12943,
#12944,#12945,#12946,#12947,#12948,#12949,#12950,#12951,#12952,#12953,#12954,
#12955,#12956,#12957,#12958,#12959,#12960,#12961,#12962,#12963,#12964,#12965,
#12966,#12967,#12968,#12969,#12970,#12971,#12972,#12973,#12974,#12975,#12976,
#12977,#12978,#12979,#12980,#12981,#12982,#12983,#12984,#12985,#12986,#12987,
#12988,#12989,#12990,#12991,#12992,#12993,#12994,#12995,#12996,#12997,#12998,
#12999,#13000,#13001,#13002,#13003,#13004,#13005,#13006,#13007,#13008,#13009,
#13010,#13011,#13012,#13013,#13014,#13015,#13016,#13017,#13018,#13019,#13020,
#13021),.UNSPECIFIED.,.F.,.F.,(4,2,2,2,2,2,2,2,2,2,2,2,2,2,2,2,2,2,2,2,
2,2,2,2,2,2,2,2,2,2,2,2,2,2,2,2,2,2,2,2,2,2,2,2,2,2,2,2,2,2,2,2,2,2,2,2,
2,2,2,2,2,2,2,2,2,2,2,2,2,2,2,2,2,2,2,2,2,2,2,2,2,2,2,2,2,2,2,2,2,2,2,2,
2,2,2,2,2,2,2,2,2,4),(-2.51343961457606,-2.50700411879925,-2.46704646714677,
-2.44191814983947,-2.42765358818164,-2.42345778919562,-2.42082515830955,
-2.41838618736802,-2.41522118302671,-2.40826685724874,-2.3577464267704,
-2.32686446612291,-2.3243328698153,-2.32218244790152,-2.32077525475688,
-2.31942380913582,-2.31740253109399,-2.31252778337271,-2.28250596247546,
-2.25389848716447,-2.23801209810173,-2.2276012878937,-2.22385498020029,
-2.22131855573529,-2.21885663492621,-2.21590493207425,-2.20850901840045,
-2.16318610321753,-2.13778920524827,-2.13006249460125,-2.1248720413167,
-2.12286525313205,-2.12147068393915,-2.12019057529134,-2.11840512372588,
-2.11374736535972,-2.07434923090019,-2.03179038556258,-2.02628881881331,
-2.02337402253571,-2.02119985331399,-2.01846578883249,-2.01380830988486,
-1.99652066761897,-1.93967124548566,-1.927148752595,-1.92441890489801,-1.92286700841356,
-1.92150805206502,-1.91975329459839,-1.91682243371769,-1.89600398338736,
-1.85074725132523,-1.83110462755919,-1.8264608122908,-1.8237295249604,-1.82131301706365,
-1.81827905865397,-1.81352646531298,-1.78537809844438,-1.73396061176384,
-1.72930379017801,-1.72578290123095,-1.72406582086938,-1.72271296400863,
-1.72111488948532,-1.71825331342435,-1.70521750918886,-1.66141040381531,
-1.63529753580209,-1.6286356378767,-1.62549007546057,-1.62306085315691,
-1.62039269663943,-1.61603716976111,-1.60178291879809,-1.54557207953828,
-1.52915157310119,-1.52621563531571,-1.52461889752026,-1.52326576389771,
-1.52154654439469,-1.51879876998948,-1.50311084355116,-1.45320575481505,
-1.43280751368249,-1.42811262893877,-1.4253698985028,-1.42295450172262,
-1.41993678749009,-1.41523849450132,-1.38872675079965,-1.34918122684277,
-1.33014676584787,-1.32710966907882,-1.32549141624457,-1.32413980419056,
-1.32244736257289,-1.31915803988056,-1.2925816857723,-1.25732799229113,
-1.25718624449385),.UNSPECIFIED.);
#109=B_SPLINE_CURVE_WITH_KNOTS('',3,(#13026,#13027,#13028,#13029,#13030,
#13031,#13032,#13033,#13034,#13035,#13036,#13037,#13038,#13039,#13040,#13041,
#13042,#13043,#13044,#13045,#13046,#13047,#13048,#13049,#13050,#13051,#13052,
#13053,#13054,#13055,#13056,#13057,#13058,#13059,#13060,#13061,#13062,#13063,
#13064,#13065,#13066,#13067,#13068,#13069,#13070,#13071,#13072,#13073,#13074,
#13075,#13076,#13077,#13078,#13079,#13080,#13081,#13082,#13083,#13084,#13085,
#13086,#13087,#13088,#13089,#13090,#13091,#13092,#13093,#13094,#13095,#13096,
#13097,#13098,#13099,#13100,#13101,#13102,#13103,#13104,#13105,#13106,#13107,
#13108,#13109,#13110,#13111,#13112,#13113,#13114,#13115,#13116,#13117,#13118,
#13119,#13120,#13121,#13122,#13123,#13124,#13125,#13126,#13127,#13128,#13129,
#13130,#13131,#13132,#13133,#13134,#13135,#13136,#13137,#13138,#13139,#13140,
#13141,#13142,#13143,#13144,#13145,#13146,#13147,#13148,#13149,#13150,#13151,
#13152,#13153,#13154,#13155,#13156,#13157,#13158,#13159,#13160,#13161,#13162,
#13163,#13164,#13165,#13166,#13167,#13168,#13169,#13170,#13171,#13172,#13173,
#13174,#13175,#13176,#13177,#13178,#13179,#13180,#13181,#13182,#13183,#13184,
#13185,#13186,#13187,#13188,#13189,#13190,#13191,#13192,#13193,#13194,#13195,
#13196,#13197,#13198,#13199,#13200,#13201,#13202,#13203,#13204,#13205,#13206,
#13207,#13208,#13209,#13210,#13211,#13212,#13213,#13214,#13215,#13216,#13217,
#13218,#13219,#13220,#13221,#13222,#13223,#13224,#13225,#13226,#13227,#13228,
#13229,#13230,#13231,#13232,#13233,#13234,#13235,#13236,#13237,#13238,#13239,
#13240,#13241,#13242,#13243,#13244,#13245,#13246,#13247,#13248,#13249,#13250,
#13251,#13252,#13253,#13254,#13255,#13256,#13257,#13258,#13259,#13260,#13261,
#13262,#13263,#13264,#13265,#13266,#13267,#13268,#13269,#13270,#13271),
 .UNSPECIFIED.,.F.,.F.,(4,2,2,2,2,2,2,2,2,2,2,2,2,2,2,2,2,2,2,2,2,2,2,2,
2,2,2,2,2,2,2,2,2,2,2,2,2,2,2,2,2,2,2,2,2,2,2,2,2,2,2,2,2,2,2,2,2,2,2,2,
2,2,2,2,2,2,2,2,2,2,2,2,2,2,2,2,2,2,2,2,2,2,2,2,2,2,2,2,2,2,2,2,2,2,2,2,
2,2,2,2,2,2,2,2,2,2,2,2,2,2,2,2,2,2,2,2,2,2,2,2,2,2,4),(-2.51376700494393,
-2.50951882086084,-2.46053664590167,-2.43229343177985,-2.42536141386723,
-2.42216526669347,-2.41972891587046,-2.41708430645807,-2.41283699457617,
-2.39953623005897,-2.3482779193926,-2.33314843911664,-2.3275405111926,-2.3247135310518,
-2.32295042109657,-2.3213343143447,-2.32132749281789,-2.32132050668485,
-2.32131334996416,-2.32130601632168,-2.32129849912296,-2.32129079137716,
-2.3212828857202,-2.32127477441211,-2.32126644925545,-2.32125790162258,
-2.32124912239502,-2.3212401019345,-2.32123083004353,-2.32122129591618,
-2.32121148808407,-2.32120139439018,-2.3211910019283,-2.32118029697447,
-2.32116926491338,-2.32115789016918,-2.31984349567252,-2.31811351985876,
-2.31533018994175,-2.29892846395731,-2.24969051023426,-2.22938937032416,
-2.22470059822666,-2.22195908171957,-2.21954333138586,-2.21652329876995,
-2.21181775690181,-2.18510154620058,-2.14573515367814,-2.12673160925154,
-2.12369540429155,-2.12207727140088,-2.12072555223376,-2.11903271606401,
-2.11574187639599,-2.08903783408751,-2.05398308729099,-2.03850012440538,
-2.02828111733017,-2.02456016183992,-2.02202830466941,-2.01956117212641,
-2.01659157210825,-2.00908682867244,-1.96610903211396,-1.93898671374315,
-1.93096633619318,-1.92562881358758,-1.92359940147936,-1.9222000298252,
-1.92092412486658,-1.91915584732139,-1.91461476245716,-1.87300896983209,
-1.83293115869864,-1.82714486219935,-1.82417075856621,-1.82175849219758,
-1.81898441300576,-1.8142709855831,-1.79559517002237,-1.74414180702794,
-1.72813833009116,-1.72522063079813,-1.72362767114012,-1.72227398087562,
-1.72054923811949,-1.71778353177524,-1.70179317254349,-1.65216836746208,
-1.63180906824576,-1.62711625548801,-1.62437373778515,-1.62195792658133,
-1.61893890118004,-1.61423702909489,-1.58763525055298,-1.54394842216482,
-1.52884986736008,-1.52597498300791,-1.52439123409069,-1.523036563021,-1.52129920111356,
-1.51849146357304,-1.50150019275957,-1.45280111895708,-1.4325806137216,
-1.42789688130584,-1.42515632969725,-1.42274023196918,-1.41971818334393,
-1.41500642915766,-1.38811896574053,-1.34890143194295,-1.32992333442592,
-1.32688781554247,-1.32526975057594,-1.32391791436567,-1.32222471322663,
-1.31893253464901,-1.29154648467702,-1.25735579703317,-1.25721314605092),
 .UNSPECIFIED.);
#110=B_SPLINE_CURVE_WITH_KNOTS('',3,(#13272,#13273,#13274,#13275,#13276,
#13277,#13278,#13279,#13280,#13281,#13282,#13283,#13284,#13285,#13286,#13287,
#13288,#13289,#13290,#13291,#13292,#13293,#13294,#13295,#13296,#13297,#13298,
#13299,#13300,#13301,#13302,#13303,#13304,#13305,#13306,#13307,#13308,#13309,
#13310,#13311,#13312,#13313,#13314,#13315,#13316,#13317,#13318,#13319,#13320,
#13321,#13322,#13323,#13324,#13325,#13326,#13327,#13328,#13329,#13330,#13331,
#13332,#13333,#13334,#13335,#13336,#13337,#13338,#13339,#13340,#13341,#13342,
#13343,#13344,#13345,#13346,#13347,#13348,#13349,#13350,#13351,#13352,#13353,
#13354,#13355,#13356,#13357,#13358,#13359,#13360,#13361,#13362,#13363,#13364,
#13365,#13366,#13367,#13368,#13369,#13370,#13371,#13372,#13373,#13374,#13375,
#13376,#13377,#13378,#13379,#13380,#13381,#13382,#13383,#13384,#13385,#13386,
#13387,#13388,#13389,#13390,#13391,#13392,#13393,#13394,#13395,#13396,#13397,
#13398,#13399,#13400,#13401,#13402,#13403,#13404,#13405,#13406,#13407,#13408,
#13409,#13410,#13411,#13412,#13413,#13414,#13415,#13416,#13417,#13418,#13419,
#13420,#13421,#13422,#13423,#13424,#13425,#13426,#13427,#13428,#13429,#13430,
#13431,#13432,#13433,#13434,#13435,#13436,#13437,#13438,#13439,#13440,#13441,
#13442,#13443,#13444,#13445,#13446,#13447,#13448,#13449,#13450,#13451,#13452,
#13453,#13454,#13455,#13456,#13457,#13458,#13459,#13460,#13461,#13462,#13463,
#13464,#13465,#13466,#13467,#13468,#13469,#13470,#13471,#13472,#13473,#13474,
#13475,#13476,#13477,#13478,#13479,#13480,#13481,#13482,#13483,#13484,#13485,
#13486,#13487,#13488,#13489,#13490,#13491,#13492,#13493,#13494,#13495,#13496,
#13497,#13498,#13499,#13500,#13501,#13502,#13503,#13504,#13505,#13506,#13507,
#13508,#13509,#13510,#13511,#13512,#13513,#13514,#13515,#13516,#13517,#13518,
#13519,#13520,#13521),.UNSPECIFIED.,.F.,.F.,(4,2,2,2,2,2,2,2,2,2,2,2,2,
2,2,2,2,2,2,2,2,2,2,2,2,2,2,2,2,2,2,2,2,2,2,2,2,2,2,2,2,2,2,2,2,2,2,2,2,
2,2,2,2,2,2,2,2,2,2,2,2,2,2,2,2,2,2,2,2,2,2,2,2,2,2,2,2,2,2,2,2,2,2,2,2,
2,2,2,2,2,2,2,2,2,2,2,2,2,2,2,2,2,2,2,2,2,2,2,2,2,2,2,2,2,2,2,2,2,2,2,2,
2,2,2,4),(-1.25718624449385,-1.23432181272649,-1.22976598265445,-1.22679172956097,
-1.22437957364868,-1.22160587769723,-1.21676918817301,-1.19402346659137,
-1.16022355147993,-1.13149350969374,-1.12820187708346,-1.12650892670364,
-1.12515727389588,-1.12353940160373,-1.12050418720247,-1.10152184785097,
-1.06223169092915,-1.03546710093895,-1.03076030774855,-1.02773993970722,
-1.02532423841764,-1.02258311834827,-1.0178958816887,-0.997617768060992,
-0.948549966039133,-0.931932334454174,-0.929139988698659,-0.927407326004779,
-0.926053142434892,-0.924466253773311,-0.921576428707393,-0.906165124988586,
-0.86003828767815,-0.836059961369632,-0.831461874734936,-0.828474623678264,
-0.826061496498789,-0.823297203262125,-0.818504001719344,-0.796521450350457,
-0.737302313453606,-0.731073098457612,-0.728846768470997,-0.727549047000138,
-0.726166641106457,-0.724228035880202,-0.719474230249166,-0.695535590368005,
-0.681607867791069,-0.640673780711772,-0.633271029246933,-0.630237319787426,
-0.627978900256045,-0.625502333925371,-0.622065053941201,-0.613742655701104,
-0.601988260361855,-0.567095524959475,-0.536346540122064,-0.531432653814182,
-0.529411445941615,-0.52802743758372,-0.526578119166187,-0.524313911346372,
-0.517197597079717,-0.505275211932711,-0.477267665615142,-0.438140639031808,
-0.433270201470152,-0.430199942586518,-0.427778939241377,-0.42506820146735,
-0.420521416268441,-0.402247534360887,-0.363623639867946,-0.334681443628133,
-0.331388931026975,-0.32969556011226,-0.328343588819775,-0.326725355915732,
-0.323689520296327,-0.304705389526956,-0.264835456090722,-0.238616623466363,
-0.233916512100262,-0.230897806361875,-0.228481746398326,-0.228432602825057,
-0.228387320658029,-0.228345588083555,-0.228307119064811,-0.228271651264636,
-0.228238944092884,-0.228208776891345,-0.228180947253649,-0.228155269479728,
-0.228131573148775,-0.228109701815023,-0.228089511809844,-0.228070871169533,
-0.228042203680407,-0.228014026252729,-0.227986327617261,-0.225103123637765,
-0.219678707888599,-0.212818064639295,-0.197377933086562,-0.162000447780933,
-0.135487182985478,-0.132197083640806,-0.130504233859789,-0.129152290567674,
-0.127533628149821,-0.124495742777054,-0.105451548106014,-0.0645853488185647,
-0.0484315952897971,-0.0371236965880628,-0.0331271481493886,-0.0305367445142057,
-0.0282310564276066,-0.025838189284329,-0.0226944322401059,-0.0147032935327984,
-0.000585061972299964),.UNSPECIFIED.);
#111=B_SPLINE_CURVE_WITH_KNOTS('',3,(#13526,#13527,#13528,#13529,#13530,
#13531,#13532,#13533,#13534,#13535,#13536,#13537,#13538,#13539,#13540,#13541,
#13542,#13543,#13544,#13545,#13546,#13547,#13548,#13549,#13550,#13551,#13552,
#13553,#13554,#13555,#13556,#13557,#13558,#13559,#13560,#13561,#13562,#13563,
#13564,#13565,#13566,#13567,#13568,#13569,#13570,#13571,#13572,#13573,#13574,
#13575,#13576,#13577,#13578,#13579,#13580,#13581,#13582,#13583,#13584,#13585,
#13586,#13587,#13588,#13589,#13590,#13591,#13592,#13593,#13594,#13595,#13596,
#13597,#13598,#13599,#13600,#13601,#13602,#13603,#13604,#13605,#13606,#13607,
#13608,#13609,#13610,#13611,#13612,#13613,#13614,#13615,#13616,#13617,#13618,
#13619,#13620,#13621,#13622,#13623,#13624,#13625,#13626,#13627,#13628,#13629,
#13630,#13631,#13632,#13633,#13634,#13635,#13636,#13637,#13638,#13639,#13640,
#13641,#13642,#13643,#13644,#13645,#13646,#13647,#13648,#13649,#13650,#13651,
#13652,#13653,#13654,#13655,#13656,#13657,#13658,#13659,#13660,#13661,#13662,
#13663,#13664,#13665,#13666,#13667,#13668,#13669,#13670,#13671,#13672,#13673,
#13674,#13675,#13676,#13677,#13678,#13679,#13680,#13681,#13682,#13683,#13684,
#13685,#13686,#13687,#13688,#13689,#13690,#13691,#13692,#13693,#13694,#13695,
#13696,#13697,#13698,#13699,#13700,#13701,#13702,#13703,#13704,#13705,#13706,
#13707,#13708,#13709,#13710,#13711,#13712,#13713,#13714,#13715,#13716,#13717,
#13718,#13719,#13720,#13721,#13722,#13723,#13724,#13725,#13726,#13727,#13728,
#13729,#13730,#13731,#13732,#13733,#13734,#13735,#13736,#13737,#13738,#13739,
#13740,#13741,#13742,#13743,#13744,#13745,#13746,#13747),.UNSPECIFIED.,
 .F.,.F.,(4,2,2,2,2,2,2,2,2,2,2,2,2,2,2,2,2,2,2,2,2,2,2,2,2,2,2,2,2,2,2,
2,2,2,2,2,2,2,2,2,2,2,2,2,2,2,2,2,2,2,2,2,2,2,2,2,2,2,2,2,2,2,2,2,2,2,2,
2,2,2,2,2,2,2,2,2,2,2,2,2,2,2,2,2,2,2,2,2,2,2,2,2,2,2,2,2,2,2,2,2,2,2,2,
2,2,2,2,2,2,2,4),(-1.25689118322759,-1.25671096155556,-1.25066039709721,
-1.20948520878915,-1.20491062352101,-1.20313712487133,-1.2018599543989,
-1.20046207327059,-1.19843965751658,-1.19314791923008,-1.18522028623814,
-1.15865150577119,-1.11497398590445,-1.10749965065631,-1.10453505784319,
-1.10206939225266,-1.09953629676943,-1.09580839389071,-1.08553717371309,
-1.06994269622606,-1.03560901004996,-1.00833240958728,-1.00504042490444,
-1.00334743610044,-1.00199583059752,-1.00037810814358,-0.997343420062909,
-0.978373648568059,-0.939151580434908,-0.912314022136519,-0.907604853576636,
-0.904583826346341,-0.902168153279766,-0.899427662031066,-0.894742989255381,
-0.874501804533818,-0.825673820371346,-0.808798892153525,-0.805995981848572,
-0.804260190475218,-0.802905808354335,-0.801321297295135,-0.798442316134587,
-0.783253095478853,-0.753093923533356,-0.713432011248414,-0.708566798631958,
-0.705498445073798,-0.703078076551615,-0.700367143047883,-0.695817851683732,
-0.677501966244538,-0.638690545643279,-0.610001738098589,-0.606710017538426,
-0.605017020098656,-0.60366532853022,-0.602047408374565,-0.59901210109803,
-0.580029064381446,-0.540736935040638,-0.513972499064096,-0.509265601671788,
-0.506245155882249,-0.503829385418153,-0.501088179338337,-0.496400776833039,
-0.476121618543464,-0.427049352990098,-0.410434549023895,-0.407642260609676,
-0.40590958908575,-0.404555369560065,-0.40296840504757,-0.400078356691766,
-0.384663685343858,-0.338511767862587,-0.314557519280654,-0.309960372522951,
-0.306973363949184,-0.304560191482653,-0.301795581799726,-0.297001152618108,
-0.274999356020909,-0.245539285514575,-0.214093563464176,-0.209207554590877,
-0.207183882719002,-0.205835679281454,-0.20442550059127,-0.202279296975025,
-0.199752659737215,-0.194972377385831,-0.183059340713377,-0.155048153012684,
-0.115924457363705,-0.111054912269187,-0.107985187527713,-0.105564587606867,
-0.102854282990023,-0.0983081798209412,-0.080036388434619,-0.0266263034238271,
-0.0178723281638256,-0.0107036920365692,-0.0083518673755166,-0.00688327863526397,
-0.005597296360091,-0.00422686397429686,-0.00239437338399666,-0.000585285094892383),
 .UNSPECIFIED.);
#112=B_SPLINE_CURVE_WITH_KNOTS('',3,(#13748,#13749,#13750,#13751,#13752,
#13753,#13754,#13755,#13756,#13757,#13758,#13759,#13760,#13761,#13762,#13763,
#13764,#13765,#13766,#13767,#13768,#13769,#13770,#13771,#13772,#13773,#13774,
#13775,#13776,#13777,#13778,#13779,#13780,#13781,#13782,#13783,#13784,#13785,
#13786,#13787,#13788,#13789,#13790,#13791,#13792,#13793,#13794,#13795,#13796,
#13797,#13798,#13799,#13800,#13801,#13802,#13803,#13804,#13805,#13806,#13807,
#13808,#13809,#13810,#13811,#13812,#13813,#13814,#13815,#13816,#13817,#13818,
#13819,#13820,#13821,#13822,#13823,#13824,#13825,#13826,#13827,#13828,#13829,
#13830,#13831,#13832,#13833,#13834,#13835,#13836,#13837,#13838,#13839,#13840,
#13841,#13842,#13843,#13844,#13845,#13846,#13847,#13848,#13849,#13850,#13851,
#13852,#13853,#13854,#13855,#13856,#13857,#13858,#13859,#13860,#13861,#13862,
#13863,#13864,#13865,#13866,#13867,#13868,#13869,#13870,#13871,#13872,#13873,
#13874,#13875,#13876,#13877,#13878,#13879,#13880,#13881,#13882,#13883,#13884,
#13885,#13886,#13887,#13888,#13889,#13890,#13891,#13892,#13893,#13894,#13895,
#13896,#13897,#13898,#13899,#13900,#13901,#13902,#13903,#13904,#13905,#13906,
#13907,#13908,#13909,#13910,#13911,#13912,#13913,#13914,#13915,#13916,#13917,
#13918,#13919,#13920,#13921,#13922,#13923,#13924,#13925,#13926,#13927,#13928,
#13929,#13930,#13931,#13932,#13933,#13934),.UNSPECIFIED.,.F.,.F.,(4,3,3,
3,3,3,3,3,3,3,3,3,3,3,3,3,3,3,3,3,3,3,3,3,3,3,3,3,3,3,3,3,3,3,3,3,3,3,3,
3,3,3,3,3,3,3,3,3,3,3,3,3,3,3,3,3,3,3,3,3,3,3,4),(128.805298797564,128.925099568478,
129.04598205521,129.156084262171,129.261064500337,129.365887762324,129.470588334727,
129.575223438936,129.679828602701,129.784439310126,129.889160442068,129.993943005775,
130.098906476961,130.152183338992,130.257163577166,130.361986839159,130.466687411564,
130.571322515774,130.675927679538,130.780538386958,130.885259518893,130.990042082592,
131.095005553766,131.148282415812,131.253262654818,131.358085917647,131.46278649089,
131.567421595939,131.67202676054,131.776637468796,131.881358601558,131.98614116608,
132.091104638063,132.144381492633,132.249361729886,132.354184990962,132.458885562461,
132.563520665773,132.668125828646,132.772736535186,132.877457666261,132.98224022911,
133.08720369946,133.140480569454,133.245460807318,133.350284068991,133.454984641061,
133.559619744928,133.66422490834,133.768835615401,133.873556746968,133.978339310294,
134.083302781091,134.136579646274,134.240837463293,134.34679324743,134.45077290342,
134.554690371446,134.658582180826,134.766057569717,134.870071282027,134.979277509208,
135.088483736389),.UNSPECIFIED.);
#113=B_SPLINE_CURVE_WITH_KNOTS('',3,(#13939,#13940,#13941,#13942,#13943,
#13944,#13945,#13946,#13947,#13948,#13949,#13950,#13951,#13952,#13953,#13954,
#13955,#13956,#13957,#13958,#13959,#13960,#13961,#13962,#13963,#13964,#13965,
#13966,#13967,#13968,#13969,#13970,#13971,#13972,#13973,#13974,#13975,#13976,
#13977,#13978,#13979,#13980,#13981,#13982,#13983,#13984,#13985,#13986,#13987,
#13988,#13989,#13990,#13991,#13992,#13993,#13994,#13995,#13996,#13997,#13998,
#13999,#14000,#14001,#14002,#14003,#14004,#14005,#14006,#14007,#14008,#14009,
#14010,#14011,#14012,#14013,#14014,#14015,#14016,#14017,#14018,#14019,#14020,
#14021,#14022,#14023,#14024,#14025,#14026,#14027,#14028,#14029,#14030,#14031,
#14032,#14033,#14034,#14035,#14036,#14037,#14038,#14039,#14040,#14041,#14042,
#14043,#14044,#14045,#14046,#14047,#14048,#14049,#14050,#14051,#14052,#14053,
#14054,#14055,#14056,#14057,#14058,#14059,#14060,#14061,#14062,#14063,#14064,
#14065,#14066,#14067,#14068,#14069,#14070,#14071,#14072,#14073,#14074,#14075,
#14076,#14077,#14078,#14079,#14080,#14081,#14082,#14083,#14084,#14085,#14086,
#14087,#14088,#14089,#14090,#14091,#14092,#14093,#14094,#14095,#14096,#14097,
#14098,#14099,#14100,#14101,#14102,#14103,#14104,#14105,#14106,#14107,#14108,
#14109,#14110,#14111,#14112,#14113,#14114,#14115,#14116,#14117,#14118,#14119,
#14120,#14121,#14122,#14123,#14124,#14125,#14126,#14127,#14128,#14129,#14130,
#14131,#14132,#14133,#14134,#14135,#14136,#14137,#14138,#14139,#14140,#14141,
#14142,#14143,#14144,#14145,#14146,#14147,#14148,#14149,#14150,#14151,#14152,
#14153,#14154),.UNSPECIFIED.,.F.,.F.,(4,2,2,2,2,2,2,2,2,2,2,2,2,2,2,2,2,
2,2,2,2,2,2,2,2,2,2,2,2,2,2,2,2,2,2,2,2,2,2,2,2,2,2,2,2,2,2,2,2,2,2,2,2,
2,2,2,2,2,2,2,2,2,2,2,2,2,2,2,2,2,2,2,2,2,2,2,2,2,2,2,2,2,2,2,2,2,2,2,2,
2,2,2,2,2,2,2,2,2,2,2,2,2,2,2,2,2,2,4),(-2.51320253931066,-2.50287632153621,
-2.49999269476239,-2.49768312658147,-2.49527430426203,-2.49248391015901,
-2.48769450544466,-2.46995109143646,-2.41385089511168,-2.40138555260747,
-2.39865980979826,-2.39710905312572,-2.39575014213638,-2.39399434132568,
-2.39105963924904,-2.37011592718344,-2.32497597339052,-2.31202115044277,
-2.30594668884389,-2.30236945828159,-2.29915574431846,-2.29675025966136,
-2.29446571714883,-2.29132511509424,-2.28499056260217,-2.23521259837668,
-2.21280395406171,-2.2056232296417,-2.20071066851767,-2.19874696748224,
-2.19736042941638,-2.1960700367412,-2.19387907785268,-2.18788906555115,
-2.14596862640986,-2.12000346906759,-2.10543782419957,-2.10121181716219,
-2.09857235025286,-2.09613525094372,-2.09298424032767,-2.08610817894176,
-2.03489016843594,-2.00454813616068,-2.00096030321405,-1.99923022322779,
-1.99787659622532,-1.99628865941446,-1.9934712508542,-1.98108139745902,
-1.97261243845498,-1.94070155955165,-1.91112041297461,-1.9040264532269,
-1.9008011001887,-1.89836090062067,-1.89605094328751,-1.89216230855972,
-1.88161578612324,-1.82105219406479,-1.80432961429153,-1.80138081352482,
-1.79978137729434,-1.79842854286192,-1.79671300830993,-1.79397734817377,
-1.77852667008295,-1.76161031874187,-1.73073990436008,-1.70824485623651,
-1.7034223418343,-1.70065171337826,-1.69823925683315,-1.69526081975989,
-1.69069135061393,-1.66737809906642,-1.62964720303596,-1.60767997776593,
-1.60312208474202,-1.60121607385071,-1.5998394994061,-1.59853285677504,
-1.59626044615774,-1.58969746879012,-1.5309160032488,-1.50897567696896,
-1.50418556920118,-1.50142219478823,-1.49900935641869,-1.4960217994714,
-1.49142194363728,-1.46739747270714,-1.42560854830984,-1.40616689497807,
-1.40311628300498,-1.40149524066759,-1.40014386083638,-1.39845492301067,
-1.39518162790263,-1.36532069691864,-1.3274477220626,-1.30935571615107,
-1.30482373422545,-1.30211675239783,-1.29969593018133,-1.29662157768381,
-1.291735922612,-1.25689118322759),.UNSPECIFIED.);
#114=B_SPLINE_CURVE_WITH_KNOTS('',3,(#14155,#14156,#14157,#14158,#14159,
#14160,#14161,#14162,#14163,#14164,#14165),.UNSPECIFIED.,.F.,.F.,(4,1,1,
1,1,1,1,1,4),(135.088484104361,135.132678723095,136.128777799915,137.124876876736,
138.120975953556,139.117075030377,140.113174107198,141.109273184018,141.371666670261),
 .UNSPECIFIED.);
#115=B_SPLINE_CURVE_WITH_KNOTS('',3,(#14170,#14171,#14172,#14173,#14174,
#14175,#14176,#14177,#14178,#14179),.UNSPECIFIED.,.F.,.F.,(4,1,1,1,1,1,
1,4),(141.371675358084,141.785434021122,142.781533097942,143.777632174763,
144.773731251584,145.769830328404,146.765929405225,147.654846025158),
 .UNSPECIFIED.);
#116=B_SPLINE_CURVE_WITH_KNOTS('',3,(#14180,#14181,#14182,#14183,#14184,
#14185,#14186,#14187,#14188,#14189,#14190,#14191,#14192,#14193,#14194,#14195,
#14196,#14197,#14198,#14199,#14200,#14201,#14202,#14203,#14204,#14205,#14206,
#14207,#14208,#14209,#14210,#14211,#14212,#14213,#14214,#14215,#14216,#14217,
#14218,#14219,#14220,#14221,#14222,#14223,#14224,#14225,#14226,#14227,#14228,
#14229,#14230,#14231,#14232,#14233,#14234,#14235,#14236,#14237,#14238,#14239,
#14240,#14241,#14242,#14243,#14244,#14245,#14246,#14247,#14248,#14249,#14250,
#14251,#14252,#14253,#14254,#14255,#14256,#14257,#14258,#14259,#14260,#14261,
#14262,#14263,#14264,#14265,#14266,#14267,#14268,#14269,#14270,#14271,#14272,
#14273,#14274,#14275,#14276,#14277,#14278,#14279,#14280,#14281,#14282,#14283,
#14284,#14285,#14286,#14287,#14288,#14289,#14290,#14291,#14292,#14293,#14294,
#14295,#14296,#14297,#14298,#14299,#14300,#14301,#14302,#14303,#14304,#14305,
#14306,#14307,#14308,#14309,#14310,#14311,#14312,#14313,#14314,#14315,#14316,
#14317,#14318,#14319,#14320,#14321,#14322,#14323,#14324,#14325,#14326,#14327,
#14328,#14329,#14330,#14331,#14332,#14333,#14334,#14335,#14336,#14337,#14338,
#14339,#14340,#14341,#14342,#14343,#14344,#14345,#14346,#14347,#14348,#14349,
#14350,#14351,#14352,#14353,#14354,#14355,#14356,#14357,#14358,#14359,#14360,
#14361,#14362,#14363,#14364,#14365,#14366,#14367,#14368,#14369,#14370,#14371,
#14372,#14373,#14374,#14375,#14376,#14377,#14378,#14379,#14380,#14381,#14382,
#14383,#14384,#14385,#14386,#14387,#14388,#14389,#14390,#14391,#14392,#14393,
#14394,#14395),.UNSPECIFIED.,.F.,.F.,(4,2,2,2,2,2,2,2,2,2,2,2,2,2,2,2,2,
2,2,2,2,2,2,2,2,2,2,2,2,2,2,2,2,2,2,2,2,2,2,2,2,2,2,2,2,2,2,2,2,2,2,2,2,
2,2,2,2,2,2,2,2,2,2,2,2,2,2,2,2,2,2,2,2,2,2,2,2,2,2,2,2,2,2,2,2,2,2,2,2,
2,2,2,2,2,2,2,2,2,2,2,2,2,2,2,2,2,2,4),(1.06702749696459,1.07316969738846,
1.07770707088996,1.08041365887283,1.08283183593376,1.08589966942507,1.09076846782211,
1.12385846889157,1.12849512758101,1.16210969520842,1.17571395237882,1.17835333713161,
1.18003871940382,1.1813894128234,1.1830123133441,1.18607065916365,1.2057327472199,
1.24862446758751,1.27143689203918,1.27598607150705,1.27895895115665,1.28137198390553,
1.28414890832231,1.28899706537762,1.31193072570234,1.34688441869337,1.37415864223013,
1.37744846191372,1.37914168114933,1.380493904015,1.38211284568512,1.38515246994505,
1.40425152330437,1.44415930257887,1.47024636851639,1.47493545036338,1.47795035489268,
1.48036550659463,1.48311011817824,1.4878136273382,1.50834427377816,1.55917481256092,
1.57389788217752,1.57659816947687,1.57830293406867,1.5796550035686,1.58126265552273,
1.58425043047079,1.60193953394739,1.62996503109149,1.66910279698706,1.67397282135017,
1.67704234054098,1.67946247365302,1.68217193286552,1.68671583748078,1.70496781130397,
1.74351087911226,1.77249917222258,1.77579028169015,1.77748296143559,1.77883449587214,
1.78045236022482,1.783487515892,1.80246398554958,1.84168311021497,1.86855896815675,
1.87326995269718,1.87629163171949,1.87870751567614,1.88144791505473,1.88613162066953,
1.90635663748937,1.95510184909357,1.97202534686489,1.97483021351245,1.97656666905203,
1.97792116205628,1.97950529482133,1.98238256472473,1.99753552905286,2.04163702341759,
2.06777405660442,2.07246296105816,2.07547778094528,2.07789288109646,2.08063745165059,
2.08511467473775,2.10277438643751,2.13944932480042,2.15466361930623,2.17119862678294,
2.17398707032581,2.17571842884612,2.17707232002611,2.1786596970405,2.18034997397262,
2.18721968582645,2.21249752401594,2.23658996480899,2.26665540963193,2.27146774281066,
2.27451997590356,2.27693849132688,2.27965877848377,2.28248115842509,2.28671622365621,
2.32340943786923),.UNSPECIFIED.);
#117=B_SPLINE_CURVE_WITH_KNOTS('',3,(#14399,#14400,#14401,#14402,#14403,
#14404),.UNSPECIFIED.,.F.,.F.,(4,1,1,4),(-4.09157007060747,-3.98439630728236,
-2.98829723046177,-2.06697924613302),.UNSPECIFIED.);
#118=B_SPLINE_CURVE_WITH_KNOTS('',3,(#14408,#14409,#14410,#14411,#14412),
 .UNSPECIFIED.,.F.,.F.,(4,1,4),(0.,0.996099076820589,1.11662023360659),
 .UNSPECIFIED.);
#119=B_SPLINE_CURVE_WITH_KNOTS('',3,(#14414,#14415,#14416,#14417,#14418,
#14419,#14420,#14421,#14422,#14423,#14424,#14425,#14426,#14427,#14428,#14429,
#14430,#14431,#14432,#14433,#14434,#14435,#14436,#14437,#14438,#14439,#14440,
#14441,#14442,#14443,#14444,#14445,#14446,#14447,#14448,#14449,#14450,#14451,
#14452,#14453,#14454,#14455,#14456,#14457,#14458,#14459,#14460,#14461,#14462,
#14463,#14464,#14465,#14466,#14467,#14468,#14469,#14470,#14471,#14472,#14473,
#14474,#14475,#14476,#14477,#14478,#14479,#14480,#14481,#14482,#14483,#14484,
#14485,#14486,#14487,#14488,#14489,#14490,#14491,#14492,#14493,#14494,#14495,
#14496,#14497,#14498,#14499,#14500,#14501,#14502,#14503,#14504,#14505,#14506,
#14507,#14508,#14509,#14510,#14511,#14512,#14513,#14514,#14515,#14516,#14517,
#14518,#14519,#14520,#14521,#14522,#14523,#14524,#14525,#14526,#14527,#14528,
#14529,#14530,#14531,#14532,#14533,#14534,#14535,#14536,#14537,#14538,#14539,
#14540,#14541,#14542,#14543,#14544,#14545,#14546,#14547,#14548,#14549,#14550,
#14551,#14552,#14553,#14554,#14555,#14556,#14557,#14558,#14559,#14560,#14561,
#14562,#14563,#14564,#14565,#14566,#14567,#14568,#14569,#14570,#14571,#14572,
#14573,#14574,#14575,#14576,#14577,#14578,#14579,#14580,#14581,#14582,#14583,
#14584,#14585,#14586,#14587,#14588,#14589,#14590,#14591,#14592,#14593,#14594,
#14595,#14596,#14597,#14598,#14599,#14600,#14601,#14602,#14603),
 .UNSPECIFIED.,.F.,.F.,(4,3,3,3,3,3,3,3,3,3,3,3,3,3,3,3,3,3,3,3,3,3,3,3,
3,3,3,3,3,3,3,3,3,3,3,3,3,3,3,3,3,3,3,3,3,3,3,3,3,3,3,3,3,3,3,3,3,3,3,3,
3,3,3,4),(1.11662023360659,1.21395960073087,1.31123941984466,1.40835533084337,
1.50542414661334,1.6024785085988,1.69990841985939,1.79708787003672,1.89464301183895,
1.99219815364118,2.09206832018503,2.19179618714873,2.2914085980286,2.39095757425931,
2.49047334616975,2.58998610368882,2.6895942510025,2.78924740690214,2.88907827446621,
2.98829723046177,3.08818590285126,3.18793562179281,3.28757488220297,3.3871537332985,
3.48670237186321,3.58625095709643,3.6858994133622,3.78559537647605,3.88547288200059,
3.98439630728237,4.08397687852573,4.18341302704854,4.28304832168035,4.38230265605514,
4.48152333465635,4.58074095905183,4.68067956531461,4.78004053948457,4.88026796179376,
4.98049538410296,5.08024179575617,5.17984583624233,5.27943941432748,5.37886540572931,
5.4782587815898,5.57764991309518,5.67738605005227,5.7769207674125,5.87675761416802,
5.97659446092355,6.07633099881174,6.17592546866135,6.2755214772967,6.37493871517028,
6.47432366735524,6.57370671833513,6.67345342318738,6.77298099142734,6.87283726458574,
6.97269353774414,7.0813231118754,7.18967359580752,7.29755728296376,7.39980554044995),
 .UNSPECIFIED.);
#120=B_SPLINE_CURVE_WITH_KNOTS('',3,(#14605,#14606,#14607,#14608,#14609,
#14610,#14611,#14612,#14613,#14614,#14615,#14616,#14617,#14618,#14619,#14620,
#14621,#14622,#14623,#14624,#14625,#14626,#14627,#14628,#14629,#14630,#14631,
#14632,#14633,#14634,#14635,#14636,#14637,#14638,#14639,#14640,#14641,#14642,
#14643,#14644,#14645,#14646,#14647,#14648,#14649,#14650,#14651,#14652,#14653,
#14654,#14655,#14656,#14657,#14658,#14659,#14660,#14661,#14662,#14663,#14664,
#14665,#14666,#14667,#14668,#14669,#14670,#14671,#14672,#14673,#14674,#14675,
#14676,#14677,#14678,#14679,#14680,#14681,#14682,#14683,#14684,#14685,#14686,
#14687,#14688,#14689,#14690,#14691,#14692,#14693,#14694,#14695,#14696,#14697,
#14698,#14699,#14700,#14701,#14702,#14703,#14704,#14705,#14706,#14707,#14708,
#14709,#14710,#14711,#14712,#14713,#14714,#14715,#14716,#14717,#14718,#14719,
#14720,#14721,#14722,#14723,#14724,#14725,#14726,#14727,#14728,#14729,#14730,
#14731,#14732,#14733,#14734,#14735,#14736,#14737,#14738,#14739,#14740,#14741,
#14742,#14743,#14744,#14745,#14746,#14747,#14748,#14749,#14750,#14751,#14752,
#14753,#14754,#14755,#14756,#14757,#14758,#14759,#14760,#14761,#14762,#14763,
#14764,#14765,#14766,#14767,#14768,#14769,#14770,#14771,#14772,#14773,#14774,
#14775,#14776,#14777,#14778,#14779,#14780,#14781,#14782,#14783,#14784,#14785,
#14786,#14787,#14788,#14789,#14790,#14791,#14792,#14793,#14794,#14795,#14796,
#14797),.UNSPECIFIED.,.F.,.F.,(4,3,3,3,3,3,3,3,3,3,3,3,3,3,3,3,3,3,3,3,
3,3,3,3,3,3,3,3,3,3,3,3,3,3,3,3,3,3,3,3,3,3,3,3,3,3,3,3,3,3,3,3,3,3,3,3,
3,3,3,3,3,3,3,3,4),(7.39980554078617,7.50127500453455,7.60280606280058,
7.70450719814795,7.80630059718374,7.90830478263615,7.96879261456473,8.06851462888085,
8.16809417032358,8.2676938604563,8.36709529233758,8.4664641421303,8.56583081537116,
8.6655960343747,8.76510671312207,8.8649992022537,8.96489169138532,9.06461014674377,
9.16418613953539,9.2637867181192,9.36318465387135,9.46255003542686,9.5619132732633,
9.66168264699895,9.7611900068315,9.8610903875187,9.96099076820591,10.0607041961592,
10.160275061418,10.259876909369,10.3592695113978,10.4586294932631,10.5579872726214,
10.6577629157227,10.7572647278683,10.8571772864474,10.9570898450265,11.0568071226611,
11.1563818918839,11.2559827706293,11.3553793797902,11.4547433987415,11.554105239685,
11.6538761602255,11.7533820527727,11.8532854873099,11.9531889218471,12.0529053877899,
12.1524793419243,12.2520804240172,12.3514762160153,12.4508394188827,12.5502004459571,
12.6499723341348,12.7494774266543,12.849382712661,12.9492879986677,13.0479544690933,
13.146491070714,13.2449296699801,13.3433020143127,13.4416647231121,13.5400212760094,
13.6384443379891,13.6829908479658),.UNSPECIFIED.);
#121=B_SPLINE_CURVE_WITH_KNOTS('',3,(#14799,#14800,#14801,#14802,#14803,
#14804,#14805,#14806,#14807,#14808,#14809,#14810,#14811,#14812,#14813,#14814,
#14815,#14816,#14817,#14818,#14819,#14820,#14821,#14822,#14823,#14824,#14825,
#14826,#14827,#14828,#14829,#14830,#14831,#14832,#14833,#14834,#14835,#14836,
#14837,#14838,#14839,#14840,#14841,#14842,#14843,#14844,#14845,#14846,#14847,
#14848,#14849,#14850,#14851,#14852,#14853,#14854,#14855,#14856,#14857,#14858,
#14859,#14860,#14861,#14862,#14863,#14864,#14865,#14866,#14867,#14868,#14869,
#14870,#14871,#14872,#14873,#14874,#14875,#14876,#14877,#14878,#14879,#14880,
#14881,#14882,#14883,#14884,#14885,#14886,#14887,#14888,#14889,#14890,#14891,
#14892,#14893,#14894,#14895,#14896,#14897,#14898,#14899,#14900,#14901,#14902,
#14903,#14904,#14905,#14906,#14907,#14908,#14909,#14910,#14911,#14912,#14913,
#14914,#14915,#14916,#14917,#14918,#14919,#14920,#14921,#14922,#14923,#14924,
#14925,#14926,#14927,#14928,#14929,#14930,#14931,#14932,#14933,#14934,#14935,
#14936,#14937,#14938,#14939,#14940,#14941,#14942,#14943,#14944,#14945,#14946,
#14947,#14948,#14949,#14950,#14951,#14952,#14953,#14954,#14955,#14956,#14957,
#14958,#14959,#14960,#14961,#14962,#14963,#14964,#14965,#14966,#14967,#14968,
#14969,#14970,#14971,#14972,#14973,#14974,#14975,#14976,#14977,#14978,#14979,
#14980,#14981,#14982,#14983,#14984,#14985,#14986,#14987,#14988),
 .UNSPECIFIED.,.F.,.F.,(4,3,3,3,3,3,3,3,3,3,3,3,3,3,3,3,3,3,3,3,3,3,3,3,
3,3,3,3,3,3,3,3,3,3,3,3,3,3,3,3,3,3,3,3,3,3,3,3,3,3,3,3,3,3,3,3,3,3,3,3,
3,3,3,4),(13.68299084831,13.8141889618991,13.9453870754883,14.045103508525,
14.1446774250973,14.2442785159987,14.3436742593052,14.4430374093747,14.5423983795991,
14.6421703227765,14.7416753490146,14.8415807506617,14.9414861523089,15.0412024277253,
15.1407761854903,15.2403773159452,15.3397728987519,15.4391358880464,15.5384966974423,
15.6382688303641,15.7377736972944,15.8376794632119,15.9375852291294,16.037301438858,
16.1368751293062,16.2364762763867,16.3358717883985,16.4352347057417,16.5345954421242,
16.6343676580806,16.7338724501227,16.8337783780363,16.93368430595,17.0334005966038,
17.1329743692339,17.232575495926,17.3319710925712,17.4313340952835,17.5306949176561,
17.6304670339347,17.7299719126177,17.8298776476941,17.9297833827706,18.0294996453416,
18.1290733896206,18.2286745233669,18.3280700912204,18.4274330650398,18.5267938584577,
18.6265660087411,18.7260708586147,18.8259766591029,18.9258824595912,19.0255987158882,
19.1251724537,19.224773589039,19.324169150001,19.4235321167842,19.5228929030299,
19.6226650613754,19.7221699038144,19.8220757201131,19.9219815364118,19.9661761551453),
 .UNSPECIFIED.);
#122=B_SPLINE_CURVE_WITH_KNOTS('',3,(#14990,#14991,#14992,#14993,#14994,
#14995,#14996,#14997,#14998,#14999,#15000,#15001,#15002,#15003,#15004,#15005,
#15006,#15007,#15008,#15009,#15010,#15011,#15012,#15013,#15014,#15015,#15016,
#15017,#15018,#15019,#15020,#15021,#15022,#15023,#15024,#15025,#15026,#15027,
#15028,#15029,#15030,#15031,#15032,#15033,#15034,#15035,#15036,#15037,#15038,
#15039,#15040,#15041,#15042,#15043,#15044,#15045,#15046,#15047,#15048,#15049,
#15050,#15051,#15052,#15053,#15054,#15055,#15056,#15057,#15058,#15059,#15060,
#15061,#15062,#15063,#15064,#15065,#15066,#15067,#15068,#15069,#15070,#15071,
#15072,#15073,#15074,#15075,#15076,#15077,#15078,#15079,#15080,#15081,#15082,
#15083,#15084,#15085,#15086,#15087,#15088,#15089,#15090,#15091,#15092,#15093,
#15094,#15095,#15096,#15097,#15098,#15099,#15100,#15101,#15102,#15103,#15104,
#15105,#15106,#15107,#15108,#15109,#15110,#15111,#15112,#15113,#15114,#15115,
#15116,#15117,#15118,#15119,#15120,#15121,#15122,#15123,#15124,#15125,#15126,
#15127,#15128,#15129,#15130,#15131,#15132,#15133,#15134,#15135,#15136,#15137,
#15138,#15139,#15140,#15141,#15142,#15143,#15144,#15145,#15146,#15147,#15148,
#15149,#15150,#15151,#15152,#15153,#15154,#15155,#15156,#15157,#15158,#15159,
#15160,#15161,#15162,#15163,#15164,#15165,#15166,#15167,#15168,#15169,#15170,
#15171,#15172,#15173,#15174,#15175,#15176,#15177,#15178,#15179),
 .UNSPECIFIED.,.F.,.F.,(4,3,3,3,3,3,3,3,3,3,3,3,3,3,3,3,3,3,3,3,3,3,3,3,
3,3,3,3,3,3,3,3,3,3,3,3,3,3,3,3,3,3,3,3,3,3,3,3,3,3,3,3,3,3,3,3,3,3,3,3,
3,3,3,4),(19.9661761554348,20.0651927431259,20.1640704476281,20.2628396467232,
20.3615508043941,20.4602352289878,20.5589241933452,20.6577132657921,20.756556096028,
20.855566502222,20.9180806132324,21.0177968761178,21.1173706206501,21.2169717543255,
21.3163673222812,21.4157302961454,21.5150910895504,21.614863239676,21.7143680893936,
21.8142738897233,21.914179690053,22.0138959525192,22.1134696966111,22.2130708303939,
22.3124663978608,22.4118293712188,22.5111901641008,22.610962314794,22.710467163953,
22.8103729654133,22.9102787668736,23.0099950308829,23.1095687765443,23.209169909938,
23.308565479027,23.4079284540233,23.5072892485576,23.6070613973418,23.7065662481709,
23.8064720459326,23.9063778436942,24.0060941069383,24.1056678518254,24.2052689854116,
24.3046645537096,24.4040275279105,24.5033883216461,24.6031604713633,24.702665321393,
24.8025711209539,24.9024769205148,25.0021931837702,25.1017669286672,25.2013680622507,
25.300763630553,25.4001266047564,25.4994873984927,25.5992595482034,25.6987643982292,
25.7986701977823,25.8985759973354,26.0135619711779,26.131461597519,26.2493612238602),
 .UNSPECIFIED.);
#123=B_SPLINE_CURVE_WITH_KNOTS('',3,(#15181,#15182,#15183,#15184,#15185,
#15186,#15187,#15188,#15189,#15190),.UNSPECIFIED.,.F.,.F.,(4,1,1,1,1,1,
1,4),(26.2493614623249,26.8946750741559,27.8907741509765,28.8868732277971,
29.8829723046177,30.8790713814383,31.8751704582589,32.5325467695045),
 .UNSPECIFIED.);
#124=B_SPLINE_CURVE_WITH_KNOTS('',3,(#15192,#15193,#15194,#15195,#15196,
#15197,#15198,#15199,#15200,#15201),.UNSPECIFIED.,.F.,.F.,(4,1,1,1,1,1,
1,4),(32.5325467695045,32.8712695350795,33.8673686119001,34.8634676887207,
35.8595667655413,36.8556658423619,37.8517649191825,38.8157320766841),
 .UNSPECIFIED.);
#125=B_SPLINE_CURVE_WITH_KNOTS('',3,(#15203,#15204,#15205,#15206,#15207,
#15208,#15209,#15210,#15211,#15212,#15213),.UNSPECIFIED.,.F.,.F.,(4,1,1,
1,1,1,1,1,4),(38.8157320766841,38.847863996003,39.8439630728236,40.8400621496442,
41.8361612264648,42.8322603032854,43.828359380106,44.8244584569266,45.0989135531719),
 .UNSPECIFIED.);
#126=B_SPLINE_CURVE_WITH_KNOTS('',3,(#15215,#15216,#15217,#15218,#15219,
#15220,#15221,#15222,#15223,#15224,#15225,#15226,#15227,#15228,#15229,#15230,
#15231,#15232,#15233,#15234,#15235,#15236,#15237,#15238,#15239,#15240,#15241,
#15242,#15243,#15244,#15245,#15246,#15247,#15248,#15249,#15250,#15251,#15252,
#15253,#15254,#15255,#15256,#15257,#15258,#15259,#15260,#15261,#15262,#15263,
#15264,#15265,#15266,#15267,#15268,#15269,#15270,#15271,#15272,#15273,#15274,
#15275,#15276,#15277,#15278,#15279,#15280,#15281,#15282,#15283,#15284,#15285,
#15286,#15287,#15288,#15289,#15290,#15291,#15292,#15293,#15294,#15295,#15296,
#15297,#15298,#15299,#15300,#15301,#15302,#15303,#15304,#15305,#15306,#15307,
#15308,#15309,#15310,#15311,#15312,#15313,#15314,#15315,#15316,#15317,#15318,
#15319,#15320,#15321,#15322,#15323,#15324,#15325,#15326,#15327,#15328,#15329,
#15330,#15331,#15332,#15333,#15334,#15335,#15336,#15337,#15338,#15339,#15340,
#15341,#15342,#15343,#15344,#15345,#15346,#15347,#15348,#15349,#15350,#15351,
#15352,#15353,#15354,#15355,#15356,#15357,#15358,#15359,#15360,#15361,#15362,
#15363,#15364,#15365,#15366,#15367,#15368,#15369,#15370,#15371,#15372,#15373,
#15374,#15375,#15376,#15377,#15378,#15379,#15380,#15381,#15382,#15383,#15384,
#15385,#15386,#15387,#15388,#15389,#15390,#15391,#15392,#15393,#15394,#15395,
#15396,#15397,#15398,#15399,#15400,#15401,#15402,#15403,#15404,#15405,#15406,
#15407),.UNSPECIFIED.,.F.,.F.,(4,3,3,3,3,3,3,3,3,3,3,3,3,3,3,3,3,3,3,3,
3,3,3,3,3,3,3,3,3,3,3,3,3,3,3,3,3,3,3,3,3,3,3,3,3,3,3,3,3,3,3,3,3,3,3,3,
3,3,3,3,3,3,3,3,4),(45.0989173838637,45.1974554529775,45.295945096918,45.3944178160819,
45.4929050849441,45.5914993213688,45.6901566383898,45.7889738889615,45.8205575337472,
45.9202737971117,46.0198475421196,46.1194486756756,46.218844244094,46.318207218415,
46.41756801227,46.5173401618445,46.6168450119913,46.7167508112796,46.8166566105678,
46.9163728739322,47.0159466189399,47.115547752496,47.2149433209143,47.3143062952352,
47.41366708909,47.5134392386646,47.6129440888115,47.7128498880999,47.8127556873883,
47.9124719507529,48.0120456957608,48.1116468293169,48.2110423977352,48.3104053720562,
48.4097661659113,48.5095383154857,48.6090431656326,48.7089489649208,48.8088547642089,
48.9085710275734,49.0081447725815,49.1077459061375,49.2071414745558,49.3065044488767,
49.4058652427315,49.505637392306,49.605142242453,49.7050480417412,49.8049538410295,
49.904670104394,50.0042438494017,50.1038449829578,50.2032405513761,50.3026035256972,
50.4019643195525,50.5017364691269,50.601241319274,50.701147118562,50.8010529178501,
50.9027101568192,51.0042053443703,51.1055352600135,51.2067678706425,51.3079249204948,
51.3821026910433),.UNSPECIFIED.);
#127=B_SPLINE_CURVE_WITH_KNOTS('',3,(#15409,#15410,#15411,#15412,#15413,
#15414,#15415,#15416,#15417,#15418,#15419,#15420,#15421,#15422,#15423,#15424,
#15425,#15426,#15427,#15428,#15429,#15430,#15431,#15432,#15433,#15434,#15435,
#15436,#15437,#15438,#15439,#15440,#15441,#15442,#15443,#15444,#15445,#15446,
#15447,#15448,#15449,#15450,#15451,#15452,#15453,#15454,#15455,#15456,#15457,
#15458,#15459,#15460,#15461,#15462,#15463,#15464,#15465,#15466,#15467,#15468,
#15469,#15470,#15471,#15472,#15473,#15474,#15475,#15476,#15477,#15478,#15479,
#15480,#15481,#15482,#15483,#15484,#15485,#15486,#15487,#15488,#15489,#15490,
#15491,#15492,#15493,#15494,#15495,#15496,#15497,#15498,#15499,#15500,#15501,
#15502,#15503,#15504,#15505,#15506,#15507,#15508,#15509,#15510,#15511,#15512,
#15513,#15514,#15515,#15516,#15517,#15518,#15519,#15520,#15521,#15522,#15523,
#15524,#15525,#15526,#15527,#15528,#15529,#15530,#15531,#15532,#15533,#15534,
#15535,#15536,#15537,#15538,#15539,#15540,#15541,#15542,#15543,#15544,#15545,
#15546,#15547,#15548,#15549,#15550,#15551,#15552,#15553,#15554,#15555,#15556,
#15557,#15558,#15559,#15560,#15561,#15562,#15563,#15564,#15565,#15566,#15567,
#15568,#15569,#15570,#15571,#15572,#15573,#15574,#15575,#15576,#15577,#15578,
#15579,#15580,#15581,#15582,#15583,#15584,#15585,#15586,#15587,#15588,#15589,
#15590,#15591,#15592,#15593,#15594,#15595,#15596,#15597,#15598),
 .UNSPECIFIED.,.F.,.F.,(4,3,3,3,3,3,3,3,3,3,3,3,3,3,3,3,3,3,3,3,3,3,3,3,
3,3,3,3,3,3,3,3,3,3,3,3,3,3,3,3,3,3,3,3,3,3,3,3,3,3,3,3,3,3,3,3,3,3,3,3,
3,3,3,4),(51.3821026914169,51.4908012816284,51.5998205885544,51.709326319515,
51.7971519946707,51.8968682580351,51.9964420030431,52.0960431365991,52.1954387050175,
52.2948016793383,52.3941624731934,52.4939346227679,52.5934394729148,52.693345272203,
52.7932510714913,52.8929673348557,52.9925410798636,53.0921422134197,53.191537781838,
53.290900756159,53.390261550014,53.4900336995885,53.5895385497354,53.6894443490237,
53.7893501483119,53.8890664116764,53.9886401566842,54.0882412902402,54.1876368586586,
54.2869998329795,54.3863606268345,54.486132776409,54.5856376265559,54.6855434258442,
54.7854492251325,54.885165488497,54.9847392335048,55.0843403670609,55.1837359354792,
55.2830989098002,55.3824597036552,55.4822318532297,55.5817367033766,55.6816425026649,
55.7815483019531,55.8812645653176,55.9808383103254,56.0804394438814,56.1798350122998,
56.2791979866208,56.3785587804758,56.4783309300503,56.5778357801972,56.6777415794854,
56.7776473787737,56.8760648306049,56.9747177265293,57.0728810226054,57.1709850818081,
57.2690618349296,57.3681183756972,57.4662860871674,57.5657870425837,57.665287998),
 .UNSPECIFIED.);
#128=B_SPLINE_CURVE_WITH_KNOTS('',3,(#15600,#15601,#15602,#15603,#15604,
#15605,#15606,#15607,#15608,#15609,#15610,#15611,#15612,#15613,#15614,#15615,
#15616,#15617,#15618,#15619,#15620,#15621,#15622,#15623,#15624,#15625,#15626,
#15627,#15628,#15629,#15630,#15631,#15632,#15633,#15634,#15635,#15636,#15637,
#15638,#15639,#15640,#15641,#15642,#15643,#15644,#15645,#15646,#15647,#15648,
#15649,#15650,#15651,#15652,#15653,#15654,#15655,#15656,#15657,#15658,#15659,
#15660,#15661,#15662,#15663,#15664,#15665,#15666,#15667,#15668,#15669,#15670,
#15671,#15672,#15673,#15674,#15675,#15676,#15677,#15678,#15679,#15680,#15681,
#15682,#15683,#15684,#15685,#15686,#15687,#15688,#15689,#15690,#15691,#15692,
#15693,#15694,#15695,#15696,#15697,#15698,#15699,#15700,#15701,#15702,#15703,
#15704,#15705,#15706,#15707,#15708,#15709,#15710,#15711,#15712,#15713,#15714,
#15715,#15716,#15717,#15718,#15719,#15720,#15721,#15722,#15723,#15724,#15725,
#15726,#15727,#15728,#15729,#15730,#15731,#15732,#15733,#15734,#15735,#15736,
#15737,#15738,#15739,#15740,#15741,#15742,#15743,#15744,#15745,#15746,#15747,
#15748,#15749,#15750,#15751,#15752,#15753,#15754,#15755,#15756,#15757,#15758,
#15759,#15760,#15761,#15762,#15763,#15764,#15765,#15766,#15767,#15768,#15769,
#15770,#15771,#15772,#15773,#15774,#15775,#15776,#15777,#15778,#15779,#15780,
#15781,#15782,#15783,#15784,#15785,#15786,#15787,#15788,#15789),
 .UNSPECIFIED.,.F.,.F.,(4,3,3,3,3,3,3,3,3,3,3,3,3,3,3,3,3,3,3,3,3,3,3,3,
3,3,3,3,3,3,3,3,3,3,3,3,3,3,3,3,3,3,3,3,3,3,3,3,3,3,3,3,3,3,3,3,3,3,3,3,
3,3,3,4),(57.6652879982229,57.7737464555943,57.8734627189586,57.9730364639664,
58.0726375975224,58.1720331659406,58.2713961402615,58.3707569341163,58.470529083691,
58.5700339338378,58.6699397331264,58.7698455324149,58.8695617957793,58.9691355407871,
59.0687366743432,59.1681322427615,59.2674952170824,59.3668560109375,59.4666281605119,
59.5661330106589,59.6660388099471,59.7659446092354,59.8656608725999,59.9652346176078,
60.0648357511638,60.1642313195822,60.2635942939031,60.3629550877582,60.4627272373327,
60.5622320874796,60.6621378867678,60.762043686056,60.8617599494205,60.9613336944283,
61.0609348279844,61.1603303964027,61.2596933707237,61.3590541645787,61.4588263141532,
61.5583311643001,61.6582369635884,61.7581427628766,61.8578590262411,61.9574327712489,
62.0570339048049,62.1564294732233,62.2557924475442,62.3551532413992,62.4549253909737,
62.5544302411206,62.6543360404089,62.7542418396972,62.8539581030616,62.9535318480695,
63.0531329816256,63.1525285500439,63.2518915243648,63.3512523182199,63.4510244677944,
63.5505293179413,63.6504351172296,63.7503409165178,63.8932777478165,63.9484733054025),
 .UNSPECIFIED.);
#129=B_SPLINE_CURVE_WITH_KNOTS('',3,(#15791,#15792,#15793,#15794,#15795,
#15796,#15797,#15798,#15799,#15800,#15801,#15802,#15803,#15804,#15805,#15806,
#15807,#15808,#15809,#15810,#15811,#15812,#15813,#15814,#15815,#15816,#15817,
#15818,#15819,#15820,#15821,#15822,#15823,#15824,#15825,#15826,#15827,#15828,
#15829,#15830,#15831,#15832,#15833,#15834,#15835,#15836,#15837,#15838,#15839,
#15840,#15841,#15842,#15843,#15844,#15845,#15846,#15847,#15848,#15849,#15850,
#15851,#15852,#15853,#15854,#15855,#15856,#15857,#15858,#15859,#15860,#15861,
#15862,#15863,#15864,#15865,#15866,#15867,#15868,#15869,#15870,#15871,#15872,
#15873,#15874,#15875,#15876,#15877,#15878,#15879,#15880,#15881,#15882,#15883,
#15884,#15885,#15886,#15887,#15888,#15889,#15890,#15891,#15892,#15893,#15894,
#15895,#15896,#15897,#15898,#15899,#15900,#15901,#15902,#15903,#15904,#15905,
#15906,#15907,#15908,#15909,#15910,#15911,#15912,#15913,#15914,#15915,#15916,
#15917,#15918,#15919,#15920,#15921,#15922,#15923,#15924,#15925,#15926,#15927,
#15928,#15929,#15930,#15931,#15932,#15933,#15934,#15935,#15936,#15937,#15938,
#15939,#15940,#15941,#15942,#15943,#15944,#15945,#15946,#15947,#15948,#15949,
#15950,#15951,#15952,#15953,#15954,#15955,#15956,#15957,#15958,#15959,#15960,
#15961,#15962,#15963,#15964,#15965,#15966,#15967,#15968,#15969,#15970,#15971,
#15972,#15973,#15974,#15975,#15976,#15977,#15978,#15979,#15980),
 .UNSPECIFIED.,.F.,.F.,(4,3,3,3,3,3,3,3,3,3,3,3,3,3,3,3,3,3,3,3,3,3,3,3,
3,3,3,3,3,3,3,3,3,3,3,3,3,3,3,3,3,3,3,3,3,3,3,3,3,3,3,3,3,3,3,3,3,3,3,3,
3,3,3,4),(63.9484733057394,64.0482191416893,64.1462266027633,64.2441857239191,
64.3421285416433,64.4432064045671,64.5412711684761,64.6438555809072,64.7464399933384,
64.8461562567029,64.9457300017107,65.0453311352667,65.1447267036851,65.2440896780061,
65.3434504718611,65.4432226214356,65.5427274715825,65.6426332708707,65.742539070159,
65.8422553335236,65.9418290785314,66.0414302120874,66.1408257805058,66.2401887548268,
66.3395495486819,66.4393216982563,66.5388265484033,66.6387323476914,66.7386381469796,
66.8383544103442,66.9379281553521,67.0375292889081,67.1369248573264,67.2362878316474,
67.3356486255025,67.4354207750769,67.5349256252239,67.634831424512,67.7347372238002,
67.8344534871647,67.9340272321724,68.0336283657284,68.1330239341468,68.2323869084678,
68.3317477023228,68.4315198518973,68.5310247020442,68.6309305013325,68.7308363006208,
68.8305525639852,68.930126308993,69.029727442549,69.1291230109673,69.2284859852882,
69.3278467791429,69.4276189287175,69.5271237788644,69.6270295781529,69.7269353774414,
69.8314472135698,69.9356740013037,70.0397314369953,70.1435751012175,70.2316586125821),
 .UNSPECIFIED.);
#130=B_SPLINE_CURVE_WITH_KNOTS('',3,(#15982,#15983,#15984,#15985,#15986,
#15987,#15988,#15989,#15990,#15991),.UNSPECIFIED.,.F.,.F.,(4,1,1,1,1,1,
1,4),(70.2316591231073,70.7230344542619,71.7191335310825,72.7152326079031,
73.7113316847237,74.7074307615443,75.7035298383649,76.5148439197617),
 .UNSPECIFIED.);
#131=B_SPLINE_CURVE_WITH_KNOTS('',3,(#15993,#15994,#15995,#15996,#15997,
#15998,#15999,#16000,#16001,#16002,#16003),.UNSPECIFIED.,.F.,.F.,(4,1,1,
1,1,1,1,1,4),(76.5148439197617,76.6996289151855,77.6957279920061,78.6918270688267,
79.6879261456473,80.6840252224679,81.6801242992884,82.676223376109,82.7980292269413),
 .UNSPECIFIED.);
#132=B_SPLINE_CURVE_WITH_KNOTS('',3,(#16005,#16006,#16007,#16008,#16009,
#16010,#16011,#16012,#16013,#16014),.UNSPECIFIED.,.F.,.F.,(4,1,1,1,1,1,
1,4),(82.7980292269413,83.6723224529296,84.6684215297502,85.6645206065708,
86.6606196833914,87.656718760212,88.6528178370326,89.0812093748789),
 .UNSPECIFIED.);
#133=B_SPLINE_CURVE_WITH_KNOTS('',3,(#16016,#16017,#16018,#16019,#16020,
#16021,#16022,#16023,#16024,#16025,#16026,#16027,#16028,#16029,#16030,#16031,
#16032,#16033,#16034,#16035,#16036,#16037,#16038,#16039,#16040,#16041,#16042,
#16043,#16044,#16045,#16046,#16047,#16048,#16049,#16050,#16051,#16052,#16053,
#16054,#16055,#16056,#16057,#16058,#16059,#16060,#16061,#16062,#16063,#16064,
#16065,#16066,#16067,#16068,#16069,#16070,#16071,#16072,#16073,#16074,#16075,
#16076,#16077,#16078,#16079,#16080,#16081,#16082,#16083,#16084,#16085,#16086,
#16087,#16088,#16089,#16090,#16091,#16092,#16093,#16094,#16095,#16096,#16097,
#16098,#16099,#16100,#16101,#16102,#16103,#16104,#16105,#16106,#16107,#16108,
#16109,#16110,#16111,#16112,#16113,#16114,#16115,#16116,#16117,#16118,#16119,
#16120,#16121,#16122,#16123,#16124,#16125,#16126,#16127,#16128,#16129,#16130,
#16131,#16132,#16133,#16134,#16135,#16136,#16137,#16138,#16139,#16140,#16141,
#16142,#16143,#16144,#16145,#16146,#16147,#16148,#16149,#16150,#16151,#16152,
#16153,#16154,#16155,#16156,#16157,#16158,#16159,#16160,#16161,#16162,#16163,
#16164,#16165,#16166,#16167,#16168,#16169,#16170,#16171,#16172,#16173,#16174,
#16175,#16176,#16177,#16178,#16179,#16180,#16181,#16182,#16183,#16184,#16185,
#16186,#16187,#16188,#16189,#16190,#16191,#16192,#16193,#16194,#16195,#16196,
#16197,#16198,#16199,#16200,#16201,#16202,#16203,#16204,#16205,#16206,#16207,
#16208),.UNSPECIFIED.,.F.,.F.,(4,3,3,3,3,3,3,3,3,3,3,3,3,3,3,3,3,3,3,3,
3,3,3,3,3,3,3,3,3,3,3,3,3,3,3,3,3,3,3,3,3,3,3,3,3,3,3,3,3,3,3,3,3,3,3,3,
3,3,3,3,3,3,3,3,4),(89.0812145341209,89.1827415934861,89.2843318214027,
89.3860935755736,89.4879486441807,89.5900145312011,89.6489169138532,89.7486331772176,
89.8482069222256,89.9478080557816,90.0472036241999,90.1465665985208,90.245927392376,
90.3456995419504,90.4452043920974,90.5451101913856,90.6450159906738,90.7447322540383,
90.844305999046,90.9439071326021,91.0433027010204,91.1426656753412,91.2420264691962,
91.3417986187707,91.4413034689177,91.541209268206,91.6411150674944,91.7408313308589,
91.8404050758667,91.9400062094227,92.039401777841,92.1387647521618,92.238125546017,
92.3378976955914,92.4374025457384,92.5373083450266,92.6372141443149,92.7369304076793,
92.8365041526871,92.9361052862431,93.0355008546614,93.1348638289824,93.2342246228377,
93.3339967724121,93.433501622559,93.5334074218472,93.6333132211355,93.7330294844999,
93.8326032295079,93.9322043630639,94.0315999314824,94.1309629058033,94.230323699658,
94.3300958492325,94.4296006993794,94.5295064986678,94.6294122979561,94.7280662758581,
94.8265905097541,94.9250168787457,95.0233771428202,95.1217282720921,95.2200733769884,
95.3184859041702,95.3643998413005),.UNSPECIFIED.);
#134=B_SPLINE_CURVE_WITH_KNOTS('',3,(#16210,#16211,#16212,#16213,#16214,
#16215,#16216,#16217,#16218,#16219,#16220,#16221,#16222,#16223,#16224,#16225,
#16226,#16227,#16228,#16229,#16230,#16231,#16232,#16233,#16234,#16235,#16236,
#16237,#16238,#16239,#16240,#16241,#16242,#16243,#16244,#16245,#16246,#16247,
#16248,#16249,#16250,#16251,#16252,#16253,#16254,#16255,#16256,#16257,#16258,
#16259,#16260,#16261,#16262,#16263,#16264,#16265,#16266,#16267,#16268,#16269,
#16270,#16271,#16272,#16273,#16274,#16275,#16276,#16277,#16278,#16279,#16280,
#16281,#16282,#16283,#16284,#16285,#16286,#16287,#16288,#16289,#16290,#16291,
#16292,#16293,#16294,#16295,#16296,#16297,#16298,#16299,#16300,#16301,#16302,
#16303,#16304,#16305,#16306,#16307,#16308,#16309,#16310,#16311,#16312,#16313,
#16314,#16315,#16316,#16317,#16318,#16319,#16320,#16321,#16322,#16323,#16324,
#16325,#16326,#16327,#16328,#16329,#16330,#16331,#16332,#16333,#16334,#16335,
#16336,#16337,#16338,#16339,#16340,#16341,#16342,#16343,#16344,#16345,#16346,
#16347,#16348,#16349,#16350,#16351,#16352,#16353,#16354,#16355,#16356,#16357,
#16358,#16359,#16360,#16361,#16362,#16363,#16364,#16365,#16366,#16367,#16368,
#16369,#16370,#16371,#16372,#16373,#16374,#16375,#16376,#16377,#16378,#16379,
#16380,#16381,#16382,#16383,#16384,#16385,#16386,#16387,#16388,#16389,#16390,
#16391,#16392,#16393,#16394,#16395,#16396,#16397,#16398,#16399),
 .UNSPECIFIED.,.F.,.F.,(4,3,3,3,3,3,3,3,3,3,3,3,3,3,3,3,3,3,3,3,3,3,3,3,
3,3,3,3,3,3,3,3,3,3,3,3,3,3,3,3,3,3,3,3,3,3,3,3,3,3,3,3,3,3,3,3,3,3,3,3,
3,3,3,4),(95.364399841631,95.4949556082039,95.6255113747767,95.7252276381412,
95.824801383149,95.924402516705,96.0237980851234,96.1231610594444,96.2225218532995,
96.3222940028739,96.4217988530209,96.5217046523091,96.6216104515973,96.7213267149618,
96.8209004599697,96.9205015935257,97.0198971619441,97.119260136265,97.21862093012,
97.3183930796945,97.4178979298414,97.5178037291297,97.6177095284179,97.7174257917823,
97.8169995367902,97.9166006703463,98.0159962387646,98.1153592130855,98.2147200069405,
98.314492156515,98.413997006662,98.5139028059502,98.6138086052385,98.7135248686029,
98.8130986136108,98.9126997471668,99.0120953155852,99.1114582899061,99.2108190837611,
99.3105912333356,99.4100960834825,99.5100018827708,99.6099076820591,99.7096239454237,
99.8091976904318,99.9087988239878,100.008194392406,100.107557366727,100.206918160583,
100.306690310157,100.406195160304,100.506100959592,100.60600675888,100.705723022244,
100.805296767252,100.904897900808,101.004293469226,101.103656443547,101.203017237402,
101.302789386976,101.402294237123,101.502200036412,101.6021058357,101.64758514848),
 .UNSPECIFIED.);
#135=B_SPLINE_CURVE_WITH_KNOTS('',3,(#16401,#16402,#16403,#16404,#16405,
#16406,#16407,#16408,#16409,#16410,#16411,#16412,#16413,#16414,#16415,#16416,
#16417,#16418,#16419,#16420,#16421,#16422,#16423,#16424,#16425,#16426,#16427,
#16428,#16429,#16430,#16431,#16432,#16433,#16434,#16435,#16436,#16437,#16438,
#16439,#16440,#16441,#16442,#16443,#16444,#16445,#16446,#16447,#16448,#16449,
#16450,#16451,#16452,#16453,#16454,#16455,#16456,#16457,#16458,#16459,#16460,
#16461,#16462,#16463,#16464,#16465,#16466,#16467,#16468,#16469,#16470,#16471,
#16472,#16473,#16474,#16475,#16476,#16477,#16478,#16479,#16480,#16481,#16482,
#16483,#16484,#16485,#16486,#16487,#16488,#16489,#16490,#16491,#16492,#16493,
#16494,#16495,#16496,#16497,#16498,#16499,#16500,#16501,#16502,#16503,#16504,
#16505,#16506,#16507,#16508,#16509,#16510,#16511,#16512,#16513,#16514,#16515,
#16516,#16517,#16518,#16519,#16520,#16521,#16522,#16523,#16524,#16525,#16526,
#16527,#16528,#16529,#16530,#16531,#16532,#16533,#16534,#16535,#16536,#16537,
#16538,#16539,#16540,#16541,#16542,#16543,#16544,#16545,#16546,#16547,#16548,
#16549,#16550,#16551,#16552,#16553,#16554,#16555,#16556,#16557,#16558,#16559,
#16560,#16561,#16562,#16563,#16564,#16565,#16566,#16567,#16568,#16569,#16570,
#16571,#16572,#16573,#16574,#16575,#16576,#16577,#16578,#16579,#16580,#16581,
#16582,#16583,#16584,#16585,#16586,#16587,#16588,#16589,#16590),
 .UNSPECIFIED.,.F.,.F.,(4,3,3,3,3,3,3,3,3,3,3,3,3,3,3,3,3,3,3,3,3,3,3,3,
3,3,3,3,3,3,3,3,3,3,3,3,3,3,3,3,3,3,3,3,3,3,3,3,3,3,3,3,3,3,3,3,3,3,3,3,
3,3,3,4),(101.647585148776,101.746584368854,101.845444892809,101.944197198785,
102.042891669239,102.141559630776,102.240232374683,102.339005330467,102.43783229681,
102.536826449131,102.598204912521,102.697921175885,102.797494920893,102.897096054449,
102.996491622867,103.095854597188,103.195215391042,103.294987540617,103.394492390764,
103.494398190052,103.594303989341,103.694020252705,103.793593997713,103.893195131269,
103.992590699688,104.091953674009,104.191314467864,104.291086617438,104.390591467585,
104.490497266874,104.590403066162,104.690119329527,104.789693074535,104.889294208091,
104.98868977651,105.088052750831,105.187413544686,105.28718569426,105.386690544408,
105.486596343695,105.586502142983,105.686218406347,105.785792151355,105.885393284911,
105.984788853329,106.08415182765,106.183512621505,106.283284771079,106.382789621226,
106.482695420514,106.582601219803,106.682317483167,106.781891228175,106.881492361731,
106.980887930149,107.08025090447,107.179611698324,107.279383847899,107.378888698046,
107.478794497335,107.578700296624,107.693554700363,107.812162458578,107.930770216793),
 .UNSPECIFIED.);
#136=B_SPLINE_CURVE_WITH_KNOTS('',3,(#16592,#16593,#16594,#16595,#16596,
#16597,#16598,#16599,#16600,#16601),.UNSPECIFIED.,.F.,.F.,(4,1,1,1,1,1,
1,4),(107.93077045566,108.574799373444,109.570898450265,110.566997527086,
111.563096603906,112.559195680727,113.555294757547,114.213955762839),
 .UNSPECIFIED.);
#137=B_SPLINE_CURVE_WITH_KNOTS('',3,(#16603,#16604,#16605,#16606,#16607,
#16608,#16609,#16610,#16611,#16612),.UNSPECIFIED.,.F.,.F.,(4,1,1,1,1,1,
1,4),(114.213955762839,114.551393834368,115.547492911189,116.543591988009,
117.53969106483,118.53579014165,119.531889218471,120.497141070019),
 .UNSPECIFIED.);
#138=B_SPLINE_CURVE_WITH_KNOTS('',3,(#16614,#16615,#16616,#16617,#16618,
#16619,#16620,#16621,#16622,#16623,#16624,#16625),.UNSPECIFIED.,.F.,.F.,
(4,2,1,1,1,1,1,1,4),(120.497141070019,120.527988295291,121.524087372112,
122.520186448933,123.516285525753,124.512384602574,125.508483679394,126.504582756215,
126.780322445093),.UNSPECIFIED.);
#139=B_SPLINE_CURVE_WITH_KNOTS('',3,(#16627,#16628,#16629,#16630,#16631,
#16632,#16633,#16634,#16635,#16636,#16637,#16638,#16639,#16640,#16641,#16642,
#16643,#16644,#16645,#16646,#16647,#16648,#16649,#16650,#16651,#16652,#16653,
#16654,#16655,#16656,#16657,#16658,#16659,#16660,#16661,#16662,#16663,#16664,
#16665,#16666,#16667,#16668,#16669,#16670,#16671,#16672,#16673,#16674,#16675,
#16676,#16677,#16678,#16679,#16680,#16681,#16682,#16683,#16684,#16685,#16686,
#16687,#16688,#16689,#16690,#16691,#16692,#16693,#16694,#16695,#16696,#16697,
#16698,#16699,#16700,#16701,#16702,#16703,#16704,#16705,#16706,#16707,#16708,
#16709,#16710,#16711,#16712,#16713,#16714,#16715,#16716,#16717,#16718,#16719,
#16720,#16721,#16722,#16723,#16724,#16725,#16726,#16727,#16728,#16729,#16730,
#16731,#16732,#16733,#16734,#16735,#16736,#16737,#16738,#16739,#16740,#16741,
#16742,#16743,#16744,#16745,#16746,#16747,#16748,#16749,#16750,#16751,#16752,
#16753,#16754,#16755,#16756,#16757,#16758,#16759,#16760,#16761,#16762,#16763,
#16764,#16765,#16766,#16767,#16768,#16769,#16770,#16771,#16772,#16773,#16774,
#16775,#16776,#16777,#16778,#16779,#16780,#16781,#16782,#16783,#16784,#16785,
#16786,#16787,#16788,#16789,#16790,#16791,#16792,#16793,#16794,#16795,#16796,
#16797,#16798,#16799,#16800,#16801,#16802,#16803,#16804,#16805,#16806,#16807,
#16808,#16809,#16810,#16811,#16812,#16813,#16814,#16815,#16816,#16817,#16818,
#16819),.UNSPECIFIED.,.F.,.F.,(4,3,3,3,3,3,3,3,3,3,3,3,3,3,3,3,3,3,3,3,
3,3,3,3,3,3,3,3,3,3,3,3,3,3,3,3,3,3,3,3,3,3,3,3,3,3,3,3,3,3,3,3,3,3,3,3,
3,3,3,3,3,3,3,3,4),(126.780326377198,126.878877284594,126.977380400159,
127.075867207474,127.17436916484,127.272978540219,127.371651503393,127.470484131865,
127.500681833036,127.600398113995,127.699971876108,127.799573005326,127.898968589554,
127.998331579165,128.097692387774,128.197464518294,128.296969381748,128.396875145802,
128.496780909856,128.596497347317,128.696071267361,128.795672357275,128.895068101716,
128.994431252039,129.093792221636,129.193564162896,129.293069186359,129.392974586518,
129.492879986677,129.592595825653,129.692169146105,129.791770385779,129.891165532297,
129.990528086646,130.089888463013,130.189661113134,130.289165556068,130.389072309782,
130.488979063497,130.588695574014,130.688269563117,130.787870635267,130.887266438695,
130.986629644111,131.085990664859,131.185762533724,131.285267598285,131.385172869301,
131.485078140318,131.584795431877,131.684370212025,131.783971087664,131.883367700396,
131.982731720144,132.082093559111,132.181864473618,132.281370357431,132.381273787285,
132.481177217139,132.582792401507,132.68424603593,132.785535467147,132.886728202003,
132.98784686251,133.063511684378),.UNSPECIFIED.);
#140=B_SPLINE_CURVE_WITH_KNOTS('',3,(#16821,#16822,#16823,#16824,#16825,
#16826,#16827,#16828,#16829,#16830,#16831,#16832,#16833,#16834,#16835,#16836,
#16837,#16838,#16839,#16840,#16841,#16842,#16843,#16844,#16845,#16846,#16847,
#16848,#16849,#16850,#16851,#16852,#16853,#16854,#16855,#16856,#16857,#16858,
#16859,#16860,#16861,#16862,#16863,#16864,#16865,#16866,#16867,#16868,#16869,
#16870,#16871,#16872,#16873,#16874,#16875,#16876,#16877,#16878,#16879,#16880,
#16881,#16882,#16883,#16884,#16885,#16886,#16887,#16888,#16889,#16890,#16891,
#16892,#16893,#16894,#16895,#16896,#16897,#16898,#16899,#16900,#16901,#16902,
#16903,#16904,#16905,#16906,#16907,#16908,#16909,#16910,#16911,#16912,#16913,
#16914,#16915,#16916,#16917,#16918,#16919,#16920,#16921,#16922,#16923,#16924,
#16925,#16926,#16927,#16928,#16929,#16930,#16931,#16932,#16933,#16934,#16935,
#16936,#16937,#16938,#16939,#16940,#16941,#16942,#16943,#16944,#16945,#16946,
#16947,#16948,#16949,#16950,#16951,#16952,#16953,#16954,#16955,#16956,#16957,
#16958,#16959,#16960,#16961,#16962,#16963,#16964,#16965,#16966,#16967,#16968,
#16969,#16970,#16971,#16972,#16973,#16974,#16975,#16976,#16977,#16978,#16979,
#16980,#16981,#16982,#16983,#16984,#16985,#16986,#16987,#16988,#16989,#16990,
#16991,#16992,#16993,#16994,#16995,#16996,#16997,#16998,#16999,#17000,#17001,
#17002,#17003,#17004,#17005,#17006,#17007,#17008,#17009,#17010),
 .UNSPECIFIED.,.F.,.F.,(4,3,3,3,3,3,3,3,3,3,3,3,3,3,3,3,3,3,3,3,3,3,3,3,
3,3,3,3,3,3,3,3,3,3,3,3,3,3,3,3,3,3,3,3,3,3,3,3,3,3,3,3,3,3,3,3,3,3,3,3,
3,3,3,4),(133.063511684756,133.172291812194,133.281396986747,133.390991808195,
133.477276293959,133.576995093555,133.6765713564,133.776171858198,133.875569882223,
133.974935283458,134.074298472429,134.174067697017,134.27357484093,134.373475105855,
134.47337537078,134.573097363914,134.672676888739,134.772276583596,134.871678010046,
134.971046858628,135.070413534876,135.170178763057,135.269689455091,135.369581951345,
135.4694744476,135.569169653751,135.668722304918,135.768328707356,135.867703245832,
135.967045260529,136.066385192976,136.166182275837,136.265666715005,136.365620119713,
136.465573524421,136.565312640281,136.664909132444,136.764504566044,136.863922464818,
136.963307564101,137.062690248756,137.162435836878,137.261961787792,137.361817194517,
137.461672601242,137.561418059226,137.661021351614,137.76061514242,137.860040889361,
137.959434210848,138.058825477927,138.158562027961,138.258097343667,138.357934510865,
138.457771678062,138.556066971266,138.654895723802,138.752936329977,138.850917784218,
138.948872116646,139.048328335374,139.146375338602,139.24653616508,139.346696991558),
 .UNSPECIFIED.);
#141=B_SPLINE_CURVE_WITH_KNOTS('',3,(#17012,#17013,#17014,#17015,#17016,
#17017),.UNSPECIFIED.,.F.,.F.,(4,1,1,4),(139.346696991558,139.453870754883,
140.449969831703,141.371287863237),.UNSPECIFIED.);
#142=B_SPLINE_CURVE_WITH_KNOTS('',3,(#17021,#17022,#17023,#17024,#17025),
 .UNSPECIFIED.,.F.,.F.,(4,1,4),(-143.438267062165,-142.442167985344,-142.321646828558),
 .UNSPECIFIED.);
#143=B_SPLINE_CURVE_WITH_KNOTS('',3,(#17027,#17028,#17029,#17030,#17031,
#17032,#17033,#17034,#17035,#17036,#17037,#17038,#17039,#17040,#17041,#17042,
#17043,#17044,#17045,#17046,#17047,#17048,#17049,#17050,#17051,#17052,#17053,
#17054,#17055,#17056,#17057,#17058,#17059,#17060,#17061,#17062,#17063,#17064,
#17065,#17066,#17067,#17068,#17069,#17070,#17071,#17072,#17073,#17074,#17075,
#17076,#17077,#17078,#17079,#17080,#17081,#17082,#17083,#17084,#17085,#17086,
#17087,#17088,#17089,#17090,#17091,#17092,#17093,#17094,#17095,#17096,#17097,
#17098,#17099,#17100,#17101,#17102,#17103,#17104,#17105,#17106,#17107,#17108,
#17109,#17110,#17111,#17112,#17113,#17114,#17115,#17116,#17117,#17118,#17119,
#17120,#17121,#17122,#17123,#17124,#17125,#17126,#17127,#17128,#17129,#17130,
#17131,#17132,#17133,#17134,#17135,#17136,#17137,#17138,#17139,#17140,#17141,
#17142,#17143,#17144,#17145,#17146,#17147,#17148,#17149,#17150,#17151,#17152,
#17153,#17154,#17155,#17156,#17157,#17158,#17159,#17160,#17161,#17162,#17163,
#17164,#17165,#17166,#17167,#17168,#17169,#17170,#17171,#17172,#17173,#17174,
#17175,#17176,#17177,#17178,#17179,#17180,#17181,#17182,#17183,#17184,#17185,
#17186,#17187,#17188,#17189,#17190,#17191,#17192,#17193,#17194,#17195,#17196,
#17197,#17198,#17199,#17200,#17201,#17202,#17203,#17204,#17205,#17206,#17207,
#17208,#17209,#17210,#17211,#17212,#17213,#17214,#17215,#17216),
 .UNSPECIFIED.,.F.,.F.,(4,3,3,3,3,3,3,3,3,3,3,3,3,3,3,3,3,3,3,3,3,3,3,3,
3,3,3,3,3,3,3,3,3,3,3,3,3,3,3,3,3,3,3,3,3,3,3,3,3,3,3,3,3,3,3,3,3,3,3,3,
3,3,3,4),(-142.321646828558,-142.224307303066,-142.127027503749,-142.029911432816,
-141.932842456695,-141.835787934027,-141.738358177651,-141.641178566955,
-141.543623737739,-141.446068908524,-141.346198822403,-141.246471036733,
-141.146858708073,-141.047309814581,-140.947794125809,-140.848281451711,
-140.748673387673,-140.6490203151,-140.549189529954,-140.449969831703,-140.350081173411,
-140.25033146897,-140.150692223606,-140.051113387881,-139.95156476499,-139.852016195714,
-139.752367755746,-139.652671809141,-139.552794320295,-139.453870754883,
-139.354290146588,-139.254853960499,-139.155218675195,-139.055964302264,
-138.956743584816,-138.857525921331,-138.757587360514,-138.658226347041,
-138.557999012552,-138.457771678062,-138.358025282948,-138.258421259161,
-138.158827676921,-138.059401702484,-137.960008343651,-137.860617229212,
-137.760881072219,-137.661346371846,-137.561509486544,-137.461672601242,
-137.361936067032,-137.262341600965,-137.162745591397,-137.06332835753,
-136.963943409428,-136.864560362603,-136.764813653057,-136.665286089106,
-136.565429806764,-136.465573524421,-136.356943941667,-136.24859344887,
-136.140709752633,-136.038461521715),.UNSPECIFIED.);
#144=B_SPLINE_CURVE_WITH_KNOTS('',3,(#17218,#17219,#17220,#17221,#17222,
#17223,#17224,#17225,#17226,#17227,#17228,#17229,#17230,#17231,#17232,#17233,
#17234,#17235,#17236,#17237,#17238,#17239,#17240,#17241,#17242,#17243,#17244,
#17245,#17246,#17247,#17248,#17249,#17250,#17251,#17252,#17253,#17254,#17255,
#17256,#17257,#17258,#17259,#17260,#17261,#17262,#17263,#17264,#17265,#17266,
#17267,#17268,#17269,#17270,#17271,#17272,#17273,#17274,#17275,#17276,#17277,
#17278,#17279,#17280,#17281,#17282,#17283,#17284,#17285,#17286,#17287,#17288,
#17289,#17290,#17291,#17292,#17293,#17294,#17295,#17296,#17297,#17298,#17299,
#17300,#17301,#17302,#17303,#17304,#17305,#17306,#17307,#17308,#17309,#17310,
#17311,#17312,#17313,#17314,#17315,#17316,#17317,#17318,#17319,#17320,#17321,
#17322,#17323,#17324,#17325,#17326,#17327,#17328,#17329,#17330,#17331,#17332,
#17333,#17334,#17335,#17336,#17337,#17338,#17339,#17340,#17341,#17342,#17343,
#17344,#17345,#17346,#17347,#17348,#17349,#17350,#17351,#17352,#17353,#17354,
#17355,#17356,#17357,#17358,#17359,#17360,#17361,#17362,#17363,#17364,#17365,
#17366,#17367,#17368,#17369,#17370,#17371,#17372,#17373,#17374,#17375,#17376,
#17377,#17378,#17379,#17380,#17381,#17382,#17383,#17384,#17385,#17386,#17387,
#17388,#17389,#17390,#17391,#17392,#17393,#17394,#17395,#17396,#17397,#17398,
#17399,#17400,#17401,#17402,#17403,#17404,#17405,#17406,#17407,#17408,#17409,
#17410),.UNSPECIFIED.,.F.,.F.,(4,3,3,3,3,3,3,3,3,3,3,3,3,3,3,3,3,3,3,3,
3,3,3,3,3,3,3,3,3,3,3,3,3,3,3,3,3,3,3,3,3,3,3,3,3,3,3,3,3,3,3,3,3,3,3,3,
3,3,3,3,3,3,3,3,4),(-136.038461521379,-135.936992047935,-135.835460979858,
-135.733759834605,-135.631966425612,-135.52996223022,-135.4694744476,-135.369752436872,
-135.270172899054,-135.17057320802,-135.071171779823,-134.971802933729,
-134.872436264197,-134.772671040843,-134.673160365789,-134.573267868285,
-134.47337537078,-134.373656915975,-134.274080923756,-134.174480345031,
-134.075082409895,-133.97571702897,-133.876353791779,-133.776584417324,
-133.677077058164,-133.577176676062,-133.477276293959,-133.377562864481,
-133.277991997674,-133.178390150107,-133.078997546483,-132.979637563009,
-132.880279782029,-132.780504140807,-132.681002327027,-132.581089772083,
-132.481177217139,-132.381459940243,-132.281885171767,-132.182284292836,
-132.082887684435,-131.983523666248,-131.884161826071,-131.784390904633,
-131.68488501285,-131.584981576584,-131.485078140318,-131.385361674423,
-131.285787720339,-131.186186638234,-131.086790846293,-130.987427643486,
-130.888066616474,-130.788294728229,-130.688789635777,-130.588884349637,
-130.488979063497,-130.390312592852,-130.291775991008,-130.193337391515,
-130.094965046952,-129.996602337919,-129.898245784786,-129.799822722568,
-129.755276214199),.UNSPECIFIED.);
#145=B_SPLINE_CURVE_WITH_KNOTS('',3,(#17412,#17413,#17414,#17415,#17416,
#17417,#17418,#17419,#17420,#17421,#17422,#17423,#17424,#17425,#17426,#17427,
#17428,#17429,#17430,#17431,#17432,#17433,#17434,#17435,#17436,#17437,#17438,
#17439,#17440,#17441,#17442,#17443,#17444,#17445,#17446,#17447,#17448,#17449,
#17450,#17451,#17452,#17453,#17454,#17455,#17456,#17457,#17458,#17459,#17460,
#17461,#17462,#17463,#17464,#17465,#17466,#17467,#17468,#17469,#17470,#17471,
#17472,#17473,#17474,#17475,#17476,#17477,#17478,#17479,#17480,#17481,#17482,
#17483,#17484,#17485,#17486,#17487,#17488,#17489,#17490,#17491,#17492,#17493,
#17494,#17495,#17496,#17497,#17498,#17499,#17500,#17501,#17502,#17503,#17504,
#17505,#17506,#17507,#17508,#17509,#17510,#17511,#17512,#17513,#17514,#17515,
#17516,#17517,#17518,#17519,#17520,#17521,#17522,#17523,#17524,#17525,#17526,
#17527,#17528,#17529,#17530,#17531,#17532,#17533,#17534,#17535,#17536,#17537,
#17538,#17539,#17540,#17541,#17542,#17543,#17544,#17545,#17546,#17547,#17548,
#17549,#17550,#17551,#17552,#17553,#17554,#17555,#17556,#17557,#17558,#17559,
#17560,#17561,#17562,#17563,#17564,#17565,#17566,#17567,#17568,#17569,#17570,
#17571,#17572,#17573,#17574,#17575,#17576,#17577,#17578,#17579,#17580,#17581,
#17582,#17583,#17584,#17585,#17586,#17587,#17588,#17589,#17590,#17591,#17592,
#17593,#17594,#17595,#17596,#17597,#17598,#17599,#17600,#17601),
 .UNSPECIFIED.,.F.,.F.,(4,3,3,3,3,3,3,3,3,3,3,3,3,3,3,3,3,3,3,3,3,3,3,3,
3,3,3,3,3,3,3,3,3,3,3,3,3,3,3,3,3,3,3,3,3,3,3,3,3,3,3,3,3,3,3,3,3,3,3,3,
3,3,3,4),(-129.755276213855,-129.624078100266,-129.492879986677,-129.393163553783,
-129.293589637355,-129.193988546418,-129.094592803258,-128.995229653337,
-128.895868683261,-128.79609673991,-128.696591713821,-128.596686311838,
-128.496780909856,-128.397064634437,-128.29749087667,-128.197889746215,
-128.098494163407,-127.999131174112,-127.899770364715,-127.799998231795,
-127.700493364865,-127.600587598951,-127.500681833036,-127.400965623265,
-127.301391932773,-127.201790785703,-127.102395273646,-127.003032356258,
-126.903671619829,-126.803899403926,-126.704394611837,-126.604488684026,
-126.504582756215,-126.404866465587,-126.305292692984,-126.205691566285,
-126.106295969667,-126.006932966982,-125.907572144637,-125.807800028326,
-125.70829514967,-125.608389414532,-125.508483679394,-125.408767416821,
-125.309193672539,-125.209592538794,-125.110196970938,-125.010833997116,
-124.911473203696,-124.811701053416,-124.71219620354,-124.612290403057,
-124.512384602574,-124.41266834627,-124.313094608452,-124.213493473115,
-124.114097912145,-124.014734945355,-123.915374159102,-123.815602000765,
-123.716097158319,-123.616191342036,-123.516285525753,-123.47209090702),
 .UNSPECIFIED.);
#146=B_SPLINE_CURVE_WITH_KNOTS('',3,(#17603,#17604,#17605,#17606,#17607,
#17608,#17609,#17610,#17611,#17612,#17613,#17614,#17615,#17616,#17617,#17618,
#17619,#17620,#17621,#17622,#17623,#17624,#17625,#17626,#17627,#17628,#17629,
#17630,#17631,#17632,#17633,#17634,#17635,#17636,#17637,#17638,#17639,#17640,
#17641,#17642,#17643,#17644,#17645,#17646,#17647,#17648,#17649,#17650,#17651,
#17652,#17653,#17654,#17655,#17656,#17657,#17658,#17659,#17660,#17661,#17662,
#17663,#17664,#17665,#17666,#17667,#17668,#17669,#17670,#17671,#17672,#17673,
#17674,#17675,#17676,#17677,#17678,#17679,#17680,#17681,#17682,#17683,#17684,
#17685,#17686,#17687,#17688,#17689,#17690,#17691,#17692,#17693,#17694,#17695,
#17696,#17697,#17698,#17699,#17700,#17701,#17702,#17703,#17704,#17705,#17706,
#17707,#17708,#17709,#17710,#17711,#17712,#17713,#17714,#17715,#17716,#17717,
#17718,#17719,#17720,#17721,#17722,#17723,#17724,#17725,#17726,#17727,#17728,
#17729,#17730,#17731,#17732,#17733,#17734,#17735,#17736,#17737,#17738,#17739,
#17740,#17741,#17742,#17743,#17744,#17745,#17746,#17747,#17748,#17749,#17750,
#17751,#17752,#17753,#17754,#17755,#17756,#17757,#17758,#17759,#17760,#17761,
#17762,#17763,#17764,#17765,#17766,#17767,#17768,#17769,#17770,#17771,#17772,
#17773,#17774,#17775,#17776,#17777,#17778,#17779,#17780,#17781,#17782,#17783,
#17784,#17785,#17786,#17787,#17788,#17789,#17790,#17791,#17792),
 .UNSPECIFIED.,.F.,.F.,(4,3,3,3,3,3,3,3,3,3,3,3,3,3,3,3,3,3,3,3,3,3,3,3,
3,3,3,3,3,3,3,3,3,3,3,3,3,3,3,3,3,3,3,3,3,3,3,3,3,3,3,3,3,3,3,3,3,3,3,3,
3,3,3,4),(-123.47209090673,-123.373074319044,-123.274196614546,-123.175427415456,
-123.07671625779,-122.978031833201,-122.879342868848,-122.780553796406,
-122.681710966175,-122.582700559986,-122.520186448933,-122.420470186047,
-122.320896441513,-122.221295307838,-122.121899739882,-122.022536766017,
-121.923175972611,-121.823403822486,-121.723898972768,-121.62399317244,
-121.524087372112,-121.424371109645,-121.324797365551,-121.225196231769,
-121.125800664301,-121.026437690942,-120.927076898058,-120.827304747366,
-120.727799898206,-120.627894096749,-120.527988295291,-120.428272031283,
-120.328698285622,-120.229097152228,-120.129701583141,-120.030338608145,
-119.930977813612,-119.831205664827,-119.731700813999,-119.631795016235,
-119.531889218471,-119.432172955226,-119.332599210339,-119.232998076753,
-119.133602508455,-119.034239534254,-118.934878740518,-118.835106590801,
-118.735601740771,-118.63569594121,-118.53579014165,-118.436073878395,-118.336500133498,
-118.236898999915,-118.137503431612,-118.038140457409,-117.938779663673,
-117.839007513962,-117.739502663937,-117.639596864383,-117.53969106483,
-117.424705090993,-117.306805464647,-117.188905838301),.UNSPECIFIED.);
#147=B_SPLINE_CURVE_WITH_KNOTS('',3,(#17794,#17795,#17796,#17797,#17798,
#17799,#17800,#17801,#17802,#17803),.UNSPECIFIED.,.F.,.F.,(4,1,1,1,1,1,
1,4),(-117.18890559984,-116.543591988009,-115.547492911189,-114.551393834368,
-113.555294757547,-112.559195680727,-111.563096603906,-110.905720292661),
 .UNSPECIFIED.);
#148=B_SPLINE_CURVE_WITH_KNOTS('',3,(#17805,#17806,#17807,#17808,#17809,
#17810,#17811,#17812,#17813,#17814),.UNSPECIFIED.,.F.,.F.,(4,1,1,1,1,1,
1,4),(-110.905720292661,-110.566997527086,-109.570898450265,-108.574799373444,
-107.578700296624,-106.582601219803,-105.586502142983,-104.622534985481),
 .UNSPECIFIED.);
#149=B_SPLINE_CURVE_WITH_KNOTS('',3,(#17816,#17817,#17818,#17819,#17820,
#17821,#17822,#17823,#17824,#17825,#17826),.UNSPECIFIED.,.F.,.F.,(4,1,1,
1,1,1,1,1,4),(-104.622534985481,-104.590403066162,-103.594303989341,-102.598204912521,
-101.6021058357,-100.60600675888,-99.6099076820591,-98.6138086052385,-98.3393535088609),
 .UNSPECIFIED.);
#150=B_SPLINE_CURVE_WITH_KNOTS('',3,(#17828,#17829,#17830,#17831,#17832,
#17833,#17834,#17835,#17836,#17837,#17838,#17839,#17840,#17841,#17842,#17843,
#17844,#17845,#17846,#17847,#17848,#17849,#17850,#17851,#17852,#17853,#17854,
#17855,#17856,#17857,#17858,#17859,#17860,#17861,#17862,#17863,#17864,#17865,
#17866,#17867,#17868,#17869,#17870,#17871,#17872,#17873,#17874,#17875,#17876,
#17877,#17878,#17879,#17880,#17881,#17882,#17883,#17884,#17885,#17886,#17887,
#17888,#17889,#17890,#17891,#17892,#17893,#17894,#17895,#17896,#17897,#17898,
#17899,#17900,#17901,#17902,#17903,#17904,#17905,#17906,#17907,#17908,#17909,
#17910,#17911,#17912,#17913,#17914,#17915,#17916,#17917,#17918,#17919,#17920,
#17921,#17922,#17923,#17924,#17925,#17926,#17927,#17928,#17929,#17930,#17931,
#17932,#17933,#17934,#17935,#17936,#17937,#17938,#17939,#17940,#17941,#17942,
#17943,#17944,#17945,#17946,#17947,#17948,#17949,#17950,#17951,#17952,#17953,
#17954,#17955,#17956,#17957,#17958,#17959,#17960,#17961,#17962,#17963,#17964,
#17965,#17966,#17967,#17968,#17969,#17970,#17971,#17972,#17973,#17974,#17975,
#17976,#17977,#17978,#17979,#17980,#17981,#17982,#17983,#17984,#17985,#17986,
#17987,#17988,#17989,#17990,#17991,#17992,#17993,#17994,#17995,#17996,#17997,
#17998,#17999,#18000,#18001,#18002,#18003,#18004,#18005,#18006,#18007,#18008,
#18009,#18010,#18011,#18012,#18013,#18014,#18015,#18016,#18017,#18018,#18019,
#18020),.UNSPECIFIED.,.F.,.F.,(4,3,3,3,3,3,3,3,3,3,3,3,3,3,3,3,3,3,3,3,
3,3,3,3,3,3,3,3,3,3,3,3,3,3,3,3,3,3,3,3,3,3,3,3,3,3,3,3,3,3,3,3,3,3,3,3,
3,3,3,3,3,3,3,3,4),(-98.3393496783013,-98.2408116091876,-98.142321965247,
-98.0438492460831,-97.9453619772209,-97.8467677407963,-97.7481104237754,
-97.6492931732037,-97.6177095284179,-97.5179932650533,-97.4184195200453,
-97.3188183864893,-97.219422818071,-97.1200598437499,-97.0206990498948,
-96.9209269003204,-96.8214220501735,-96.7215162508854,-96.6216104515973,
-96.5218941882327,-96.4223204432247,-96.3227193096687,-96.2233237412504,
-96.1239607669294,-96.0245999730744,-95.9248278235,-95.8253229733531,-95.7254171740649,
-95.6255113747767,-95.5257951114123,-95.4262213664045,-95.3266202328485,
-95.2272246644301,-95.1278616901092,-95.0285008962541,-94.9287287466796,
-94.8292238965327,-94.7293180972444,-94.6294122979561,-94.5296960345917,
-94.4301222895839,-94.3305211560279,-94.2311255876095,-94.1317626132885,
-94.0324018194335,-93.932629669859,-93.8331248197122,-93.7332190204238,
-93.6333132211355,-93.5335969577712,-93.4340232127631,-93.3344220792071,
-93.2350265107889,-93.1356635364681,-93.0363027426131,-92.9365305930386,
-92.8370257428917,-92.7371199436033,-92.6372141443149,-92.5355569053459,
-92.4340617177943,-92.3327318021511,-92.2314991915218,-92.1303421416695,
-92.0561643711217),.UNSPECIFIED.);
#151=B_SPLINE_CURVE_WITH_KNOTS('',3,(#18022,#18023,#18024,#18025,#18026,
#18027,#18028,#18029,#18030,#18031,#18032,#18033,#18034,#18035,#18036,#18037,
#18038,#18039,#18040,#18041,#18042,#18043,#18044,#18045,#18046,#18047,#18048,
#18049,#18050,#18051,#18052,#18053,#18054,#18055,#18056,#18057,#18058,#18059,
#18060,#18061,#18062,#18063,#18064,#18065,#18066,#18067,#18068,#18069,#18070,
#18071,#18072,#18073,#18074,#18075,#18076,#18077,#18078,#18079,#18080,#18081,
#18082,#18083,#18084,#18085,#18086,#18087,#18088,#18089,#18090,#18091,#18092,
#18093,#18094,#18095,#18096,#18097,#18098,#18099,#18100,#18101,#18102,#18103,
#18104,#18105,#18106,#18107,#18108,#18109,#18110,#18111,#18112,#18113,#18114,
#18115,#18116,#18117,#18118,#18119,#18120,#18121,#18122,#18123,#18124,#18125,
#18126,#18127,#18128,#18129,#18130,#18131,#18132,#18133,#18134,#18135,#18136,
#18137,#18138,#18139,#18140,#18141,#18142,#18143,#18144,#18145,#18146,#18147,
#18148,#18149,#18150,#18151,#18152,#18153,#18154,#18155,#18156,#18157,#18158,
#18159,#18160,#18161,#18162,#18163,#18164,#18165,#18166,#18167,#18168,#18169,
#18170,#18171,#18172,#18173,#18174,#18175,#18176,#18177,#18178,#18179,#18180,
#18181,#18182,#18183,#18184,#18185,#18186,#18187,#18188,#18189,#18190,#18191,
#18192,#18193,#18194,#18195,#18196,#18197,#18198,#18199,#18200,#18201,#18202,
#18203,#18204,#18205,#18206,#18207,#18208,#18209,#18210,#18211),
 .UNSPECIFIED.,.F.,.F.,(4,3,3,3,3,3,3,3,3,3,3,3,3,3,3,3,3,3,3,3,3,3,3,3,
3,3,3,3,3,3,3,3,3,3,3,3,3,3,3,3,3,3,3,3,3,3,3,3,3,3,3,3,3,3,3,3,3,3,3,3,
3,3,3,4),(-92.0561643707481,-91.9474657805367,-91.8384464736106,-91.7289407426503,
-91.6411150674944,-91.5413988041299,-91.441825059122,-91.342223925566,-91.2428283571476,
-91.1434653828266,-91.0441045889715,-90.9443324393971,-90.8448275892501,
-90.744921789962,-90.6450159906738,-90.5452997273093,-90.4457259823015,
-90.3461248487454,-90.2467292803271,-90.1473663060061,-90.0480055121511,
-89.9482333625766,-89.8487285124297,-89.7488227131414,-89.6489169138532,
-89.5492006504887,-89.4496269054809,-89.3500257719249,-89.2506302035065,
-89.1512672291856,-89.0519064353306,-88.9521342857561,-88.8526294356091,
-88.7527236363209,-88.6528178370326,-88.5531015736681,-88.4535278286602,
-88.3539266951042,-88.2545311266858,-88.1551681523649,-88.0558073585099,
-87.9560352089354,-87.8565303587885,-87.7566245595002,-87.656718760212,
-87.5570024968475,-87.4574287518397,-87.3578276182837,-87.2584320498653,
-87.1590690755444,-87.0597082816894,-86.9599361321149,-86.860431281968,
-86.7605254826797,-86.6606196833914,-86.5622022315602,-86.4635493356358,
-86.3653860395597,-86.267281980357,-86.1692052272356,-86.070148686468,-85.9719809749976,
-85.8724800195813,-85.772979064165),.UNSPECIFIED.);
#152=B_SPLINE_CURVE_WITH_KNOTS('',3,(#18213,#18214,#18215,#18216,#18217,
#18218,#18219,#18220,#18221,#18222,#18223,#18224,#18225,#18226,#18227,#18228,
#18229,#18230,#18231,#18232,#18233,#18234,#18235,#18236,#18237,#18238,#18239,
#18240,#18241,#18242,#18243,#18244,#18245,#18246,#18247,#18248,#18249,#18250,
#18251,#18252,#18253,#18254,#18255,#18256,#18257,#18258,#18259,#18260,#18261,
#18262,#18263,#18264,#18265,#18266,#18267,#18268,#18269,#18270,#18271,#18272,
#18273,#18274,#18275,#18276,#18277,#18278,#18279,#18280,#18281,#18282,#18283,
#18284,#18285,#18286,#18287,#18288,#18289,#18290,#18291,#18292,#18293,#18294,
#18295,#18296,#18297,#18298,#18299,#18300,#18301,#18302,#18303,#18304,#18305,
#18306,#18307,#18308,#18309,#18310,#18311,#18312,#18313,#18314,#18315,#18316,
#18317,#18318,#18319,#18320,#18321,#18322,#18323,#18324,#18325,#18326,#18327,
#18328,#18329,#18330,#18331,#18332,#18333,#18334,#18335,#18336,#18337,#18338,
#18339,#18340,#18341,#18342,#18343,#18344,#18345,#18346,#18347,#18348,#18349,
#18350,#18351,#18352,#18353,#18354,#18355,#18356,#18357,#18358,#18359,#18360,
#18361,#18362,#18363,#18364,#18365,#18366,#18367,#18368,#18369,#18370,#18371,
#18372,#18373,#18374,#18375,#18376,#18377,#18378,#18379,#18380,#18381,#18382,
#18383,#18384,#18385,#18386,#18387,#18388,#18389,#18390,#18391,#18392,#18393,
#18394,#18395,#18396,#18397,#18398,#18399,#18400,#18401,#18402),
 .UNSPECIFIED.,.F.,.F.,(4,3,3,3,3,3,3,3,3,3,3,3,3,3,3,3,3,3,3,3,3,3,3,3,
3,3,3,3,3,3,3,3,3,3,3,3,3,3,3,3,3,3,3,3,3,3,3,3,3,3,3,3,3,3,3,3,3,3,3,3,
3,3,3,4),(-85.7729790639421,-85.6645206065708,-85.5648043432062,-85.4652305981982,
-85.3656294646422,-85.2662338962237,-85.1668709219025,-85.0675101280473,
-84.9677379784731,-84.8682331283259,-84.7683273290381,-84.6684215297502,
-84.5687052663858,-84.4691315213779,-84.3695303878219,-84.2701348194036,
-84.1707718450827,-84.0714110512278,-83.9716389016532,-83.8721340515064,
-83.772228252218,-83.6723224529296,-83.5726061895651,-83.4730324445573,
-83.3734313110012,-83.2740357425829,-83.1746727682619,-83.0753119744069,
-82.9755398248324,-82.8760349746855,-82.7761291753972,-82.676223376109,
-82.5765071127445,-82.4769333677366,-82.3773322341806,-82.2779366657622,
-82.1785736914413,-82.0792128975862,-81.9794407480118,-81.8799358978648,
-81.7800300985766,-81.6801242992884,-81.580408035924,-81.4808342909161,
-81.3812331573601,-81.2818375889418,-81.1824746146209,-81.0831138207659,
-80.9833416711914,-80.8838368210445,-80.7839310217562,-80.6840252224679,
-80.5843089591034,-80.4847352140955,-80.3851340805394,-80.2857385121211,
-80.1863755378002,-80.0870147439451,-79.9872425943706,-79.8877377442237,
-79.7878319449355,-79.6879261456473,-79.5449893143448,-79.4897937567626),
 .UNSPECIFIED.);
#153=B_SPLINE_CURVE_WITH_KNOTS('',3,(#18404,#18405,#18406,#18407,#18408,
#18409,#18410,#18411,#18412,#18413,#18414,#18415,#18416,#18417,#18418,#18419,
#18420,#18421,#18422,#18423,#18424,#18425,#18426,#18427,#18428,#18429,#18430,
#18431,#18432,#18433,#18434,#18435,#18436,#18437,#18438,#18439,#18440,#18441,
#18442,#18443,#18444,#18445,#18446,#18447,#18448,#18449,#18450,#18451,#18452,
#18453,#18454,#18455,#18456,#18457,#18458,#18459,#18460,#18461,#18462,#18463,
#18464,#18465,#18466,#18467,#18468,#18469,#18470,#18471,#18472,#18473,#18474,
#18475,#18476,#18477,#18478,#18479,#18480,#18481,#18482,#18483,#18484,#18485,
#18486,#18487,#18488,#18489,#18490,#18491,#18492,#18493,#18494,#18495,#18496,
#18497,#18498,#18499,#18500,#18501,#18502,#18503,#18504,#18505,#18506,#18507,
#18508,#18509,#18510,#18511,#18512,#18513,#18514,#18515,#18516,#18517,#18518,
#18519,#18520,#18521,#18522,#18523,#18524,#18525,#18526,#18527,#18528,#18529,
#18530,#18531,#18532,#18533,#18534,#18535,#18536,#18537,#18538,#18539,#18540,
#18541,#18542,#18543,#18544,#18545,#18546,#18547,#18548,#18549,#18550,#18551,
#18552,#18553,#18554,#18555,#18556,#18557,#18558,#18559,#18560,#18561,#18562,
#18563,#18564,#18565,#18566,#18567,#18568,#18569,#18570,#18571,#18572,#18573,
#18574,#18575,#18576,#18577,#18578,#18579,#18580,#18581,#18582,#18583,#18584,
#18585,#18586,#18587,#18588,#18589,#18590,#18591,#18592,#18593),
 .UNSPECIFIED.,.F.,.F.,(4,3,3,3,3,3,3,3,3,3,3,3,3,3,3,3,3,3,3,3,3,3,3,3,
3,3,3,3,3,3,3,3,3,3,3,3,3,3,3,3,3,3,3,3,3,3,3,3,3,3,3,3,3,3,3,3,3,3,3,3,
3,3,3,4),(-79.4897937564256,-79.3900479204758,-79.2920404594018,-79.1940813382461,
-79.0961385205218,-78.995060657598,-78.896995893689,-78.7944114812578,-78.6918270688267,
-78.5921108054622,-78.4925370604542,-78.3929359268982,-78.2935403584798,
-78.194177384159,-78.0948165903039,-77.9950444407295,-77.8955395905825,
-77.7956337912943,-77.6957279920061,-77.5960117286416,-77.4964379836338,
-77.3968368500778,-77.2974412816595,-77.1980783073386,-77.0987175134835,
-76.998945363909,-76.8994405137621,-76.7995347144738,-76.6996289151855,
-76.599912651821,-76.5003389068132,-76.4007377732572,-76.3013422048388,
-76.2019792305179,-76.1026184366628,-76.0028462870883,-75.9033414369415,
-75.8034356376532,-75.7035298383649,-75.6038135750004,-75.5042398299924,
-75.4046386964364,-75.3052431280181,-75.2058801536972,-75.1065193598425,
-75.0067472102679,-74.9072423601209,-74.8073365608326,-74.7074307615443,
-74.6077144981799,-74.5081407531721,-74.408539619616,-74.3091440511978,
-74.209781076877,-74.1104202830217,-74.0106481334472,-73.9111432833001,
-73.8112374840119,-73.7113316847237,-73.6068198485953,-73.5025930608617,
-73.3985356251701,-73.294691960948,-73.206608449583),.UNSPECIFIED.);
#154=B_SPLINE_CURVE_WITH_KNOTS('',3,(#18595,#18596,#18597,#18598,#18599,
#18600,#18601,#18602,#18603,#18604),.UNSPECIFIED.,.F.,.F.,(4,1,1,1,1,1,
1,4),(-73.2066079390623,-72.7152326079031,-71.7191335310825,-70.7230344542619,
-69.7269353774414,-68.7308363006208,-67.7347372238002,-66.9234231424034),
 .UNSPECIFIED.);
#155=B_SPLINE_CURVE_WITH_KNOTS('',3,(#18606,#18607,#18608,#18609,#18610,
#18611,#18612,#18613,#18614,#18615,#18616),.UNSPECIFIED.,.F.,.F.,(4,1,1,
1,1,1,1,1,4),(-66.9234231424034,-66.7386381469796,-65.742539070159,-64.7464399933384,
-63.7503409165178,-62.7542418396972,-61.7581427628766,-60.762043686056,
-60.6402378352238),.UNSPECIFIED.);
#156=B_SPLINE_CURVE_WITH_KNOTS('',3,(#18618,#18619,#18620,#18621,#18622,
#18623,#18624,#18625,#18626,#18627),.UNSPECIFIED.,.F.,.F.,(4,1,1,1,1,1,
1,4),(-60.6402378352238,-59.7659446092355,-58.7698455324149,-57.7737464555943,
-56.7776473787737,-55.7815483019531,-54.7854492251325,-54.3570576872367),
 .UNSPECIFIED.);
#157=B_SPLINE_CURVE_WITH_KNOTS('',3,(#18629,#18630,#18631,#18632,#18633,
#18634,#18635,#18636,#18637,#18638,#18639,#18640,#18641,#18642,#18643,#18644,
#18645,#18646,#18647,#18648,#18649,#18650,#18651,#18652,#18653,#18654,#18655,
#18656,#18657,#18658,#18659,#18660,#18661,#18662,#18663,#18664,#18665,#18666,
#18667,#18668,#18669,#18670,#18671,#18672,#18673,#18674,#18675,#18676,#18677,
#18678,#18679,#18680,#18681,#18682,#18683,#18684,#18685,#18686,#18687,#18688,
#18689,#18690,#18691,#18692,#18693,#18694,#18695,#18696,#18697,#18698,#18699,
#18700,#18701,#18702,#18703,#18704,#18705,#18706,#18707,#18708,#18709,#18710,
#18711,#18712,#18713,#18714,#18715,#18716,#18717,#18718,#18719,#18720,#18721,
#18722,#18723,#18724,#18725,#18726,#18727,#18728,#18729,#18730,#18731,#18732,
#18733,#18734,#18735,#18736,#18737,#18738,#18739,#18740,#18741,#18742,#18743,
#18744,#18745,#18746,#18747,#18748,#18749,#18750,#18751,#18752,#18753,#18754,
#18755,#18756,#18757,#18758,#18759,#18760,#18761,#18762,#18763,#18764,#18765,
#18766,#18767,#18768,#18769,#18770,#18771,#18772,#18773,#18774,#18775,#18776,
#18777,#18778,#18779,#18780,#18781,#18782,#18783,#18784,#18785,#18786,#18787,
#18788,#18789,#18790,#18791,#18792,#18793,#18794,#18795,#18796,#18797,#18798,
#18799,#18800,#18801,#18802,#18803,#18804,#18805,#18806,#18807,#18808,#18809,
#18810,#18811,#18812,#18813,#18814,#18815,#18816,#18817,#18818,#18819,#18820,
#18821),.UNSPECIFIED.,.F.,.F.,(4,3,3,3,3,3,3,3,3,3,3,3,3,3,3,3,3,3,3,3,
3,3,3,3,3,3,3,3,3,3,3,3,3,3,3,3,3,3,3,3,3,3,3,3,3,3,3,3,3,3,3,3,3,3,3,3,
3,3,3,3,3,3,3,3,4),(-54.3570525280442,-54.2555254686791,-54.1539352407624,
-54.0521734865916,-53.9503184179844,-53.8482525309639,-53.7893501483119,
-53.6896338849475,-53.5900601399395,-53.4904590063835,-53.3910634379651,
-53.2917004636443,-53.1923396697892,-53.0925675202148,-52.9930626700678,
-52.8931568707795,-52.7932510714913,-52.6935348081268,-52.5939610631188,
-52.4943599295628,-52.3949643611444,-52.2956013868235,-52.1962405929686,
-52.0964684433942,-51.9969635932472,-51.8970577939589,-51.7971519946707,
-51.6974357313063,-51.5978619862985,-51.4982608527425,-51.3988652843241,
-51.2995023100033,-51.2001415161481,-51.1003693665736,-51.0008645164266,
-50.9009587171384,-50.8010529178501,-50.7013366544856,-50.6017629094778,
-50.5021617759218,-50.4027662075034,-50.3034032331824,-50.2040424393273,
-50.1042702897528,-50.0047654396059,-49.9048596403177,-49.8049538410295,
-49.705237577665,-49.6056638326575,-49.5060626991014,-49.4066671306832,
-49.3073041563622,-49.2079433625071,-49.1081712129326,-49.0086663627857,
-48.9087605634973,-48.8088547642089,-48.710200786307,-48.611676552411,-48.5132501834196,
-48.4148899193455,-48.3165387900736,-48.2181936851774,-48.1197811579957,
-48.0738672208646),.UNSPECIFIED.);
#158=B_SPLINE_CURVE_WITH_KNOTS('',3,(#18823,#18824,#18825,#18826,#18827,
#18828,#18829,#18830,#18831,#18832,#18833,#18834,#18835,#18836,#18837,#18838,
#18839,#18840,#18841,#18842,#18843,#18844,#18845,#18846,#18847,#18848,#18849,
#18850,#18851,#18852,#18853,#18854,#18855,#18856,#18857,#18858,#18859,#18860,
#18861,#18862,#18863,#18864,#18865,#18866,#18867,#18868,#18869,#18870,#18871,
#18872,#18873,#18874,#18875,#18876,#18877,#18878,#18879,#18880,#18881,#18882,
#18883,#18884,#18885,#18886,#18887,#18888,#18889,#18890,#18891,#18892,#18893,
#18894,#18895,#18896,#18897,#18898,#18899,#18900,#18901,#18902,#18903,#18904,
#18905,#18906,#18907,#18908,#18909,#18910,#18911,#18912,#18913,#18914,#18915,
#18916,#18917,#18918,#18919,#18920,#18921,#18922,#18923,#18924,#18925,#18926,
#18927,#18928,#18929,#18930,#18931,#18932,#18933,#18934,#18935,#18936,#18937,
#18938,#18939,#18940,#18941,#18942,#18943,#18944,#18945,#18946,#18947,#18948,
#18949,#18950,#18951,#18952,#18953,#18954,#18955,#18956,#18957,#18958,#18959,
#18960,#18961,#18962,#18963,#18964,#18965,#18966,#18967,#18968,#18969,#18970,
#18971,#18972,#18973,#18974,#18975,#18976,#18977,#18978,#18979,#18980,#18981,
#18982,#18983,#18984,#18985,#18986,#18987,#18988,#18989,#18990,#18991,#18992,
#18993,#18994,#18995,#18996,#18997,#18998,#18999,#19000,#19001,#19002,#19003,
#19004,#19005,#19006,#19007,#19008,#19009,#19010,#19011,#19012),
 .UNSPECIFIED.,.F.,.F.,(4,3,3,3,3,3,3,3,3,3,3,3,3,3,3,3,3,3,3,3,3,3,3,3,
3,3,3,3,3,3,3,3,3,3,3,3,3,3,3,3,3,3,3,3,3,3,3,3,3,3,3,3,3,3,3,3,3,3,3,3,
3,3,3,4),(-48.0738672205341,-47.9433114539612,-47.8127556873884,-47.7130394240239,
-47.613465679016,-47.51386454546,-47.4144689770416,-47.3151060027206,-47.2157452088656,
-47.1159730592911,-47.0164682091442,-46.916562409856,-46.8166566105678,
-46.7169403472033,-46.6173666021954,-46.5177654686394,-46.418369900221,
-46.3190069259001,-46.2196461320451,-46.1198739824706,-46.0203691323237,
-45.9204633330354,-45.8205575337472,-45.7208412703827,-45.6212675253749,
-45.5216663918188,-45.4222708234005,-45.3229078490796,-45.2235470552246,
-45.1237749056501,-45.0242700555032,-44.9243642562149,-44.8244584569266,
-44.7247421935621,-44.6251684485543,-44.5255673149982,-44.4261717465799,
-44.326808772259,-44.2274479784039,-44.1276758288294,-44.0281709786825,
-43.9282651793943,-43.828359380106,-43.7286431167415,-43.6290693717336,
-43.5294682381776,-43.4300726697592,-43.3307096954383,-43.2313489015833,
-43.1315767520088,-43.0320719018619,-42.9321661025737,-42.8322603032854,
-42.7325440399209,-42.6329702949131,-42.533369161357,-42.4339735929387,
-42.3346106186178,-42.2352498247627,-42.1354776751882,-42.0359728250413,
-41.936067025753,-41.8361612264648,-41.790681913685),.UNSPECIFIED.);
#159=B_SPLINE_CURVE_WITH_KNOTS('',3,(#19014,#19015,#19016,#19017,#19018,
#19019,#19020,#19021,#19022,#19023,#19024,#19025,#19026,#19027,#19028,#19029,
#19030,#19031,#19032,#19033,#19034,#19035,#19036,#19037,#19038,#19039,#19040,
#19041,#19042,#19043,#19044,#19045,#19046,#19047,#19048,#19049,#19050,#19051,
#19052,#19053,#19054,#19055,#19056,#19057,#19058,#19059,#19060,#19061,#19062,
#19063,#19064,#19065,#19066,#19067,#19068,#19069,#19070,#19071,#19072,#19073,
#19074,#19075,#19076,#19077,#19078,#19079,#19080,#19081,#19082,#19083,#19084,
#19085,#19086,#19087,#19088,#19089,#19090,#19091,#19092,#19093,#19094,#19095,
#19096,#19097,#19098,#19099,#19100,#19101,#19102,#19103,#19104,#19105,#19106,
#19107,#19108,#19109,#19110,#19111,#19112,#19113,#19114,#19115,#19116,#19117,
#19118,#19119,#19120,#19121,#19122,#19123,#19124,#19125,#19126,#19127,#19128,
#19129,#19130,#19131,#19132,#19133,#19134,#19135,#19136,#19137,#19138,#19139,
#19140,#19141,#19142,#19143,#19144,#19145,#19146,#19147,#19148,#19149,#19150,
#19151,#19152,#19153,#19154,#19155,#19156,#19157,#19158,#19159,#19160,#19161,
#19162,#19163,#19164,#19165,#19166,#19167,#19168,#19169,#19170,#19171,#19172,
#19173,#19174,#19175,#19176,#19177,#19178,#19179,#19180,#19181,#19182,#19183,
#19184,#19185,#19186,#19187,#19188,#19189,#19190,#19191,#19192,#19193,#19194,
#19195,#19196,#19197,#19198,#19199,#19200,#19201,#19202,#19203),
 .UNSPECIFIED.,.F.,.F.,(4,3,3,3,3,3,3,3,3,3,3,3,3,3,3,3,3,3,3,3,3,3,3,3,
3,3,3,3,3,3,3,3,3,3,3,3,3,3,3,3,3,3,3,3,3,3,3,3,3,3,3,3,3,3,3,3,3,3,3,3,
3,3,3,4),(-41.790681913389,-41.6916826933112,-41.5928221693564,-41.4940698633804,
-41.3953753929266,-41.2967074313893,-41.198034687483,-41.0992617316987,
-41.0004347653562,-40.9014406130349,-40.8400621496442,-40.7403458862797,
-40.640772141272,-40.5411710077159,-40.4417754392976,-40.3424124649767,
-40.2430516711217,-40.1432795215472,-40.0437746714003,-39.9438688721119,
-39.8439630728236,-39.7442468094591,-39.6446730644513,-39.5450719308952,
-39.4456763624769,-39.346313388156,-39.246952594301,-39.1471804447265,-39.0476755945796,
-38.9477697952913,-38.847863996003,-38.7481477326385,-38.648573987631,-38.5489728540749,
-38.4495772856566,-38.3502143113355,-38.2508535174804,-38.1510813679059,
-38.051576517759,-37.9516707184707,-37.8517649191824,-37.752048655818,-37.6524749108102,
-37.5528737772542,-37.4534782088358,-37.3541152345149,-37.2547544406597,
-37.1549822910853,-37.0554774409384,-36.9555716416501,-36.8556658423619,
-36.7559495789976,-36.6563758339897,-36.5567747004336,-36.4573791320155,
-36.3580161576947,-36.2586553638398,-36.1588832142652,-36.0593783641184,
-35.9594725648298,-35.8595667655413,-35.7447123618031,-35.6261046035863,
-35.5074968453696),.UNSPECIFIED.);
#160=B_SPLINE_CURVE_WITH_KNOTS('',3,(#19205,#19206,#19207,#19208,#19209,
#19210,#19211,#19212,#19213,#19214),.UNSPECIFIED.,.F.,.F.,(4,1,1,1,1,1,
1,4),(-35.5074966065054,-34.8634676887207,-33.8673686119001,-32.8712695350795,
-31.8751704582589,-30.8790713814383,-29.8829723046177,-29.2243112993258),
 .UNSPECIFIED.);
#161=B_SPLINE_CURVE_WITH_KNOTS('',3,(#19216,#19217,#19218,#19219,#19220,
#19221,#19222,#19223,#19224,#19225),.UNSPECIFIED.,.F.,.F.,(4,1,1,1,1,1,
1,4),(-29.2243112993258,-28.8868732277971,-27.8907741509765,-26.894675074156,
-25.8985759973354,-24.9024769205148,-23.9063778436942,-22.9411259921462),
 .UNSPECIFIED.);
#162=B_SPLINE_CURVE_WITH_KNOTS('',3,(#19227,#19228,#19229,#19230,#19231,
#19232,#19233,#19234,#19235,#19236,#19237),.UNSPECIFIED.,.F.,.F.,(4,1,1,
1,1,1,1,1,4),(-22.9411259921462,-22.9102787668736,-21.914179690053,-20.9180806132324,
-19.9219815364118,-18.9258824595912,-17.9297833827706,-16.93368430595,-16.6579446169396),
 .UNSPECIFIED.);
#163=B_SPLINE_CURVE_WITH_KNOTS('',3,(#19239,#19240,#19241,#19242,#19243,
#19244,#19245,#19246,#19247,#19248,#19249,#19250,#19251,#19252,#19253,#19254,
#19255,#19256,#19257,#19258,#19259,#19260,#19261,#19262,#19263,#19264,#19265,
#19266,#19267,#19268,#19269,#19270,#19271,#19272,#19273,#19274,#19275,#19276,
#19277,#19278,#19279,#19280,#19281,#19282,#19283,#19284,#19285,#19286,#19287,
#19288,#19289,#19290,#19291,#19292,#19293,#19294,#19295,#19296,#19297,#19298,
#19299,#19300,#19301,#19302,#19303,#19304,#19305,#19306,#19307,#19308,#19309,
#19310,#19311,#19312,#19313,#19314,#19315,#19316,#19317,#19318,#19319,#19320,
#19321,#19322,#19323,#19324,#19325,#19326,#19327,#19328,#19329,#19330,#19331,
#19332,#19333,#19334,#19335,#19336,#19337,#19338,#19339,#19340,#19341,#19342,
#19343,#19344,#19345,#19346,#19347,#19348,#19349,#19350,#19351,#19352,#19353,
#19354,#19355,#19356,#19357,#19358,#19359,#19360,#19361,#19362,#19363,#19364,
#19365,#19366,#19367,#19368,#19369,#19370,#19371,#19372,#19373,#19374,#19375,
#19376,#19377,#19378,#19379,#19380,#19381,#19382,#19383,#19384,#19385,#19386,
#19387,#19388,#19389,#19390,#19391,#19392,#19393,#19394,#19395,#19396,#19397,
#19398,#19399,#19400,#19401,#19402,#19403,#19404,#19405,#19406,#19407,#19408,
#19409,#19410,#19411,#19412,#19413,#19414,#19415,#19416,#19417,#19418,#19419,
#19420,#19421,#19422,#19423,#19424,#19425,#19426,#19427,#19428,#19429,#19430,
#19431),.UNSPECIFIED.,.F.,.F.,(4,3,3,3,3,3,3,3,3,3,3,3,3,3,3,3,3,3,3,3,
3,3,3,3,3,3,3,3,3,3,3,3,3,3,3,3,3,3,3,3,3,3,3,3,3,3,3,3,3,3,3,3,3,3,3,3,
3,3,3,3,3,3,3,3,4),(-16.6579406849666,-16.5593897775357,-16.4608866619369,
-16.3623998545879,-16.2638978971885,-16.1652885217759,-16.0666155585702,
-15.9677829300662,-15.9375852291295,-15.8378689481712,-15.7382951860584,
-15.6386940568397,-15.5392984726109,-15.4399354829983,-15.3405746743875,
-15.2408025438679,-15.1412976804118,-15.0413919163603,-14.9414861523089,
-14.8417697149956,-14.7421957951011,-14.6425947051495,-14.5431989608577,
-14.4438358106844,-14.3444748412367,-14.2447028997996,-14.1451978764835,
-14.0452924759859,-13.9453870754883,-13.8456712362277,-13.7460979154923,
-13.6464966758892,-13.5471015290883,-13.4477389744586,-13.3483785978117,
-13.2486059480257,-13.1491015048194,-13.0491947517435,-12.9492879986677,
-12.8495714882222,-12.7499974991886,-12.650396427021,-12.5510006236563,
-12.4516374183018,-12.3522763976134,-12.2525045286719,-12.1529994641636,
-12.0530941930054,-11.9531889218471,-11.8534716310433,-11.7538968516564,
-11.6542959758276,-11.5548993638604,-11.4555353448774,-11.356173506674,
-11.2564025912621,-11.1568967082028,-11.0569932766146,-10.9570898450265,
-10.8554746586855,-10.754021022291,-10.6527315891179,-10.5515388523147,
-10.4504201898901,-10.3747553777871),.UNSPECIFIED.);
#164=B_SPLINE_CURVE_WITH_KNOTS('',3,(#19432,#19433,#19434,#19435,#19436,
#19437,#19438,#19439,#19440,#19441,#19442,#19443,#19444,#19445,#19446,#19447,
#19448,#19449,#19450,#19451,#19452,#19453,#19454,#19455,#19456,#19457,#19458,
#19459,#19460,#19461,#19462,#19463,#19464,#19465,#19466,#19467,#19468,#19469,
#19470,#19471,#19472,#19473,#19474,#19475,#19476,#19477,#19478,#19479,#19480,
#19481,#19482,#19483,#19484,#19485,#19486,#19487,#19488,#19489,#19490,#19491,
#19492,#19493,#19494,#19495,#19496,#19497,#19498,#19499,#19500,#19501,#19502,
#19503,#19504,#19505,#19506,#19507,#19508,#19509,#19510,#19511,#19512,#19513,
#19514,#19515,#19516,#19517,#19518,#19519,#19520,#19521,#19522,#19523,#19524,
#19525,#19526,#19527,#19528,#19529,#19530,#19531,#19532,#19533,#19534,#19535,
#19536,#19537,#19538,#19539,#19540,#19541,#19542,#19543,#19544,#19545,#19546,
#19547,#19548,#19549,#19550,#19551,#19552,#19553,#19554,#19555,#19556,#19557,
#19558,#19559,#19560,#19561,#19562,#19563,#19564,#19565,#19566,#19567,#19568,
#19569,#19570,#19571,#19572,#19573,#19574,#19575,#19576,#19577,#19578,#19579,
#19580,#19581,#19582,#19583,#19584,#19585,#19586,#19587,#19588,#19589,#19590,
#19591,#19592,#19593,#19594,#19595,#19596,#19597,#19598,#19599,#19600,#19601,
#19602,#19603,#19604,#19605,#19606,#19607,#19608,#19609,#19610,#19611,#19612,
#19613,#19614,#19615,#19616,#19617,#19618,#19619,#19620,#19621),
 .UNSPECIFIED.,.F.,.F.,(4,3,3,3,3,3,3,3,3,3,3,3,3,3,3,3,3,3,3,3,3,3,3,3,
3,3,3,3,3,3,3,3,3,3,3,3,3,3,3,3,3,3,3,3,3,3,3,3,3,3,3,3,3,3,3,3,3,3,3,3,
3,3,3,4),(-10.3747553774094,-10.2659752484022,-10.1568700723105,-10.0472752494143,
-9.96099076820591,-9.86127196929943,-9.7616957071339,-9.66209520516533,
-9.56269718179088,-9.46333178119533,-9.36396859284967,-9.26419936748358,
-9.16469222415936,-9.06479195777234,-8.96489169138532,-8.86516970189676,
-8.76559018074002,-8.66599048496811,-8.56658906221728,-8.46722021733717,
-8.36785354478904,-8.26808831223296,-8.16857762385655,-8.06868511921064,
-7.96879261456473,-7.8690973998874,-7.76954474017978,-7.66993833987533,
-7.5705637928849,-7.47122176970325,-7.37188182881078,-7.27208475604412,
-7.17260030861201,-7.07264692317808,-6.97269353774414,-6.87295442623608,
-6.77335793838362,-6.67376250370111,-6.57434460910662,-6.47495951394585,
-6.37557683335036,-6.27583124024365,-6.17630529319603,-6.07644987705978,
-5.97659446092354,-5.87684901969211,-5.77724574417183,-5.67765194916322,
-5.57822621924204,-5.47883291479406,-5.37944166475022,-5.2797050945884,
-5.18016979573384,-5.0803325899184,-4.98049538410295,-4.88220005204375,
-4.78337130436421,-4.68533065927096,-4.58734916614617,-4.48939479490125,
-4.38993861382781,-4.29189157221189,-4.19173082140968,-4.09157007060747),
 .UNSPECIFIED.);
#165=B_SPLINE_CURVE_WITH_KNOTS('',3,(#19624,#19625,#19626,#19627,#19628,
#19629,#19630,#19631,#19632,#19633,#19634,#19635,#19636,#19637,#19638,#19639,
#19640,#19641,#19642,#19643,#19644,#19645,#19646,#19647,#19648,#19649,#19650,
#19651,#19652,#19653,#19654,#19655,#19656,#19657,#19658,#19659,#19660,#19661,
#19662,#19663,#19664,#19665,#19666,#19667,#19668,#19669,#19670,#19671,#19672,
#19673,#19674,#19675,#19676,#19677,#19678,#19679,#19680,#19681,#19682,#19683,
#19684,#19685,#19686,#19687,#19688,#19689,#19690,#19691,#19692,#19693,#19694,
#19695,#19696,#19697,#19698,#19699,#19700,#19701,#19702,#19703,#19704,#19705,
#19706,#19707,#19708,#19709,#19710,#19711,#19712,#19713,#19714,#19715,#19716,
#19717,#19718,#19719,#19720,#19721,#19722,#19723,#19724,#19725,#19726,#19727,
#19728,#19729,#19730,#19731,#19732,#19733,#19734,#19735,#19736,#19737,#19738,
#19739,#19740,#19741,#19742,#19743,#19744,#19745,#19746,#19747,#19748,#19749,
#19750,#19751,#19752,#19753,#19754,#19755,#19756,#19757,#19758,#19759,#19760,
#19761,#19762,#19763,#19764,#19765,#19766,#19767,#19768,#19769,#19770,#19771,
#19772,#19773,#19774,#19775,#19776,#19777,#19778,#19779,#19780,#19781,#19782,
#19783,#19784,#19785,#19786,#19787,#19788,#19789,#19790,#19791,#19792,#19793,
#19794,#19795,#19796,#19797,#19798,#19799,#19800,#19801,#19802,#19803,#19804,
#19805,#19806,#19807,#19808,#19809,#19810,#19811,#19812,#19813,#19814,#19815,
#19816,#19817,#19818,#19819,#19820,#19821,#19822,#19823),.UNSPECIFIED.,
 .F.,.F.,(4,2,2,2,2,2,2,2,2,2,2,2,2,2,2,2,2,2,2,2,2,2,2,2,2,2,2,2,2,2,2,
2,2,2,2,2,2,2,2,2,2,2,2,2,2,2,2,2,2,2,2,2,2,2,2,2,2,2,2,2,2,2,2,2,2,2,2,
2,2,2,2,2,2,2,2,2,2,2,2,2,2,2,2,2,2,2,2,2,2,2,2,2,2,2,2,2,2,2,2,4),(0.00326162500843006,
0.0197447762864837,0.0748215617595025,0.082167278784108,0.0854722927311191,
0.0879597576891903,0.0906299556293424,0.0948557198684813,0.107639883892953,
0.151800459018261,0.178902896427261,0.182192364140908,0.18387015633938,
0.183879116759064,0.183888299241087,0.183897711707281,0.183907362460959,
0.183917260204829,0.183927414073413,0.183937833665262,0.183948529061159,
0.183959510853069,0.18397079019248,0.18398237881444,0.183994289087449,0.184006534032961,
0.184019127396874,0.184032083688368,0.185383199046984,0.187067363254308,
0.190340194813029,0.218062962634009,0.257340175901016,0.275744767436072,
0.280315400158962,0.2830400089683,0.285473338279774,0.288559280984999,0.293454778705634,
0.332862991654633,0.361103634370691,0.373011519743452,0.380126153845839,
0.382391447113787,0.383841767871193,0.385218283606201,0.387225981320361,
0.392102170469598,0.421882741364194,0.457578467176283,0.475570096991801,
0.480073813086898,0.482762335967425,0.485165431345914,0.488215332912887,
0.493057333654311,0.53194547082417,0.559769077621238,0.57825267981081,0.581253242296325,
0.582855641916501,0.584203409276343,0.585898403562848,0.58856480988963,
0.602607510633657,0.608628735611976,0.652983968945658,0.674690687177921,
0.679476468698024,0.682243905683431,0.684664267023071,0.687666412674625,
0.692299156560563,0.71695516502572,0.757831396980101,0.777100723342141,
0.780154965497359,0.781781398879197,0.78313716291058,0.784832370830203,
0.788127593165175,0.817294661810435,0.855680716458636,0.873892619328436,
0.878435414468737,0.881145769002038,0.883567689344995,0.886640832883721,
0.891519267651087,0.930057646863374,0.957446404750408,0.976344496235866,
0.979376527435769,0.980993504510696,0.982344337096749,0.984036172650702,
0.987326764415839,1.01665603120223,1.05497305173704,1.06702749696459),
 .UNSPECIFIED.);
#166=B_SPLINE_CURVE_WITH_KNOTS('',3,(#19826,#19827,#19828,#19829,#19830,
#19831,#19832,#19833,#19834,#19835,#19836,#19837,#19838,#19839,#19840,#19841,
#19842,#19843,#19844,#19845,#19846,#19847,#19848,#19849,#19850,#19851,#19852,
#19853,#19854,#19855,#19856,#19857,#19858,#19859,#19860,#19861,#19862,#19863,
#19864,#19865,#19866,#19867,#19868,#19869,#19870,#19871,#19872,#19873,#19874,
#19875,#19876,#19877,#19878,#19879,#19880,#19881,#19882,#19883,#19884,#19885,
#19886,#19887,#19888,#19889,#19890,#19891,#19892,#19893,#19894,#19895,#19896,
#19897,#19898,#19899,#19900,#19901,#19902,#19903,#19904,#19905,#19906,#19907,
#19908,#19909,#19910,#19911,#19912,#19913,#19914,#19915,#19916,#19917,#19918,
#19919,#19920,#19921,#19922,#19923,#19924,#19925,#19926,#19927,#19928,#19929,
#19930,#19931,#19932,#19933,#19934,#19935,#19936,#19937,#19938,#19939,#19940,
#19941,#19942,#19943,#19944,#19945,#19946,#19947,#19948,#19949),
 .UNSPECIFIED.,.F.,.F.,(4,3,3,3,3,3,3,3,3,3,3,3,3,3,3,3,3,3,3,3,3,3,3,3,
3,3,3,3,3,3,3,3,3,3,3,3,3,3,3,3,3,4),(147.65485471872,147.762028482045,
147.86721043816,147.972234768624,148.077134483648,148.181967416618,148.286768802862,
148.391573832499,148.496485101084,148.601455688331,148.706601951883,148.758127558866,
148.863259229857,148.968236566764,149.073094308716,149.177888396139,149.282654092532,
149.387426619453,149.492310360179,149.597256212211,149.702382262756,149.754226635687,
149.858063290691,149.961742205202,150.065302377591,150.168799882304,150.272271688643,
150.375754725542,150.47936423613,150.583042333312,150.686924471371,150.750325712507,
150.858239782028,150.96926290794,151.076819947692,151.184275590721,151.291658671096,
151.398997929083,151.506351328449,151.613712019336,151.721144432213,151.746424789328),
 .UNSPECIFIED.);
#167=B_SPLINE_CURVE_WITH_KNOTS('',3,(#20538,#20539,#20540,#20541,#20542,
#20543,#20544,#20545,#20546,#20547,#20548,#20549,#20550,#20551,#20552,#20553,
#20554,#20555,#20556,#20557,#20558,#20559,#20560,#20561,#20562,#20563,#20564,
#20565,#20566,#20567,#20568,#20569,#20570,#20571,#20572,#20573,#20574,#20575,
#20576,#20577,#20578,#20579,#20580,#20581,#20582,#20583,#20584,#20585,#20586,
#20587,#20588,#20589,#20590,#20591,#20592,#20593,#20594,#20595,#20596,#20597,
#20598,#20599,#20600,#20601,#20602,#20603,#20604,#20605,#20606,#20607,#20608,
#20609,#20610,#20611,#20612,#20613,#20614,#20615,#20616,#20617,#20618,#20619,
#20620,#20621,#20622,#20623,#20624,#20625),.UNSPECIFIED.,.F.,.F.,(4,3,3,
3,3,3,3,3,3,3,3,3,3,3,3,3,3,3,3,3,3,3,3,3,3,3,3,3,3,4),(0.,0.0182760710704149,
0.0437675064709697,0.0695752992456494,0.0922813564527724,0.0963438741865412,
0.121479543983109,0.146526999164012,0.170952555575599,0.182419474302491,
0.186963208615901,0.211099004300551,0.234533760957442,0.251900460808682,
0.26514437268587,0.271415138183839,0.275123593425889,0.298667119795758,
0.322419773257956,0.345934625047122,0.351073300043322,0.35531942417871,
0.359377579094087,0.382316439597603,0.402792093527263,0.408417580703764,
0.413280341911519,0.435488471747807,0.457053381724928,0.463803050843696),
 .UNSPECIFIED.);
#168=B_SPLINE_CURVE_WITH_KNOTS('',3,(#20627,#20628,#20629,#20630,#20631,
#20632,#20633,#20634,#20635,#20636,#20637,#20638,#20639,#20640,#20641,#20642,
#20643,#20644,#20645,#20646,#20647,#20648,#20649,#20650,#20651,#20652,#20653,
#20654,#20655,#20656,#20657,#20658,#20659,#20660,#20661,#20662,#20663,#20664,
#20665,#20666,#20667,#20668,#20669,#20670,#20671,#20672,#20673,#20674,#20675,
#20676,#20677,#20678,#20679,#20680,#20681,#20682,#20683,#20684,#20685,#20686,
#20687,#20688,#20689,#20690,#20691,#20692,#20693,#20694,#20695,#20696,#20697,
#20698,#20699,#20700,#20701,#20702,#20703,#20704,#20705,#20706,#20707,#20708,
#20709,#20710,#20711),.UNSPECIFIED.,.F.,.F.,(4,3,3,3,3,3,3,3,3,3,3,3,3,
3,3,3,3,3,3,3,3,3,3,3,3,3,3,3,4),(-0.463803050843718,-0.448740022185204,
-0.42691444385268,-0.414669408555542,-0.410232646093364,-0.387935224132788,
-0.365010556573471,-0.359638840893696,-0.355551191051294,-0.351346727838988,
-0.327878176942996,-0.304134002765552,-0.280552762497995,-0.273242198114603,
-0.268716587605523,-0.244288506390758,-0.235180056184415,-0.211343912259743,
-0.187507768335072,-0.183690135280684,-0.15932822702224,-0.134515626743572,
-0.109408117315328,-0.0938532048355855,-0.0899591209447907,-0.0642123177659208,
-0.0384373539397261,-0.0132154939304623,-1.37208636376373E-15),
 .UNSPECIFIED.);
#169=B_SPLINE_CURVE_WITH_KNOTS('',3,(#20712,#20713,#20714,#20715),
 .UNSPECIFIED.,.F.,.F.,(4,4),(-0.0135998802120258,0.),.UNSPECIFIED.);
#170=B_SPLINE_CURVE_WITH_KNOTS('',3,(#21305,#21306,#21307,#21308,#21309,
#21310,#21311,#21312,#21313,#21314,#21315,#21316,#21317,#21318,#21319,#21320,
#21321,#21322,#21323,#21324,#21325,#21326,#21327,#21328,#21329,#21330,#21331,
#21332,#21333,#21334,#21335,#21336,#21337,#21338,#21339,#21340,#21341,#21342,
#21343,#21344,#21345,#21346,#21347,#21348,#21349,#21350,#21351,#21352,#21353,
#21354,#21355,#21356,#21357,#21358,#21359,#21360,#21361,#21362,#21363,#21364,
#21365,#21366,#21367,#21368,#21369,#21370,#21371,#21372,#21373,#21374,#21375,
#21376,#21377,#21378,#21379,#21380,#21381,#21382,#21383,#21384,#21385,#21386,
#21387,#21388,#21389,#21390,#21391,#21392,#21393,#21394,#21395),
 .UNSPECIFIED.,.F.,.F.,(4,3,3,3,3,3,3,3,3,3,3,3,3,3,3,3,3,3,3,3,3,3,3,3,
3,3,3,3,3,3,4),(0.,0.0150138269319462,0.036520890660569,0.0587157842271369,
0.0697076727300594,0.0762008005980358,0.0816663983792169,0.104427855536438,
0.127790613405416,0.151113577304524,0.159780223723126,0.163861468767013,
0.187890149415679,0.211826173958714,0.227871101166216,0.242490967649561,
0.246618252277857,0.250650056860218,0.27416492806894,0.29836373674207,0.323030301871278,
0.329929523699832,0.335709402506641,0.339916278287732,0.365088975678724,
0.390432981304092,0.397923686724778,0.402696895452255,0.428440535010322,
0.453950365417961,0.461788964899747),.UNSPECIFIED.);
#171=B_SPLINE_CURVE_WITH_KNOTS('',3,(#21396,#21397,#21398,#21399),
 .UNSPECIFIED.,.F.,.F.,(4,4),(0.,0.0135996993161776),.UNSPECIFIED.);
#172=B_SPLINE_CURVE_WITH_KNOTS('',3,(#21400,#21401,#21402,#21403,#21404,
#21405,#21406,#21407,#21408,#21409,#21410,#21411,#21412,#21413,#21414,#21415,
#21416,#21417,#21418,#21419,#21420,#21421,#21422,#21423,#21424,#21425,#21426,
#21427,#21428,#21429,#21430,#21431,#21432,#21433,#21434,#21435,#21436,#21437,
#21438,#21439,#21440,#21441,#21442,#21443,#21444,#21445,#21446,#21447,#21448,
#21449,#21450,#21451,#21452,#21453,#21454,#21455,#21456,#21457,#21458,#21459,
#21460,#21461,#21462,#21463,#21464,#21465,#21466,#21467,#21468,#21469,#21470,
#21471,#21472,#21473,#21474,#21475,#21476,#21477,#21478,#21479,#21480,#21481,
#21482,#21483,#21484,#21485,#21486,#21487,#21488,#21489,#21490),
 .UNSPECIFIED.,.F.,.F.,(4,3,3,3,3,3,3,3,3,3,3,3,3,3,3,3,3,3,3,3,3,3,3,3,
3,3,3,3,3,3,4),(-0.461788964899773,-0.443595824964341,-0.417881602474246,
-0.405040573218592,-0.399033269720178,-0.394779666370722,-0.369467283426724,
-0.344172275666879,-0.340434254998593,-0.335819056172879,-0.331683328772696,
-0.306946125658135,-0.282481738829071,-0.258728029909401,-0.251428002001961,
-0.247028273677602,-0.243317649896853,-0.219840949155418,-0.211223388199231,
-0.187163181376808,-0.163852594642498,-0.158770548393032,-0.135417929772648,
-0.112049986589736,-0.0891501996726069,-0.0803321462983234,-0.076617754044123,
-0.0541541414655251,-0.0320539914425208,-0.0106610814724787,0.),
 .UNSPECIFIED.);
#173=B_SPLINE_CURVE_WITH_KNOTS('',3,(#21553,#21554,#21555,#21556,#21557,
#21558,#21559,#21560,#21561,#21562),.UNSPECIFIED.,.F.,.F.,(4,2,2,2,4),(0.304370745831088,
0.340749860871315,0.378176848018549,0.416877357705943,0.456616383722292),
 .UNSPECIFIED.);
#174=B_SPLINE_CURVE_WITH_KNOTS('',3,(#21571,#21572,#21573,#21574,#21575,
#21576,#21577,#21578,#21579,#21580,#21581,#21582),.UNSPECIFIED.,.F.,.F.,
(4,2,2,2,2,4),(-0.956034309409163,-0.919797905610199,-0.883592147057887,
-0.844404551538294,-0.805088366243444,-0.793069564297015),.UNSPECIFIED.);
#175=B_SPLINE_CURVE_WITH_KNOTS('',3,(#21606,#21607,#21608,#21609,#21610,
#21611,#21612,#21613,#21614,#21615,#21616,#21617),.UNSPECIFIED.,.F.,.F.,
(4,2,2,2,2,4),(-0.793069564419585,-0.765429318917777,-0.726356329910807,
-0.690453978752587,-0.655278338273468,-0.628541412295733),.UNSPECIFIED.);
#176=B_SPLINE_CURVE_WITH_KNOTS('',3,(#21620,#21621,#21622,#21623,#21624,
#21625,#21626,#21627,#21628,#21629),.UNSPECIFIED.,.F.,.F.,(4,2,2,2,4),(0.152125107939884,
0.191864133956234,0.230564643643628,0.267991630790861,0.304370745831088),
 .UNSPECIFIED.);
#177=B_SPLINE_CURVE_WITH_KNOTS('',5,(#21645,#21646,#21647,#21648,#21649,
#21650,#21651,#21652,#21653,#21654,#21655,#21656,#21657,#21658,#21659,#21660,
#21661,#21662,#21663,#21664,#21665,#21666,#21667,#21668,#21669,#21670,#21671,
#21672,#21673,#21674,#21675,#21676,#21677,#21678,#21679,#21680,#21681,#21682,
#21683,#21684,#21685,#21686,#21687,#21688,#21689,#21690,#21691,#21692,#21693,
#21694,#21695,#21696,#21697,#21698,#21699),.UNSPECIFIED.,.F.,.F.,(6,1,1,
1,1,1,1,1,1,1,1,1,1,1,1,1,1,1,1,1,1,1,1,1,1,1,1,1,1,1,1,1,1,1,1,1,1,1,1,
1,1,1,1,1,1,1,1,1,1,1,6),(0.,0.02,0.04,0.06,0.08,0.1,0.12,0.14,0.16,0.18,
0.2,0.22,0.24,0.26,0.28,0.3,0.32,0.34,0.36,0.38,0.4,0.42,0.44,0.46,0.48,
0.5,0.52,0.54,0.56,0.58,0.6,0.62,0.64,0.66,0.68,0.7,0.72,0.74,0.76,0.78,
0.8,0.82,0.84,0.86,0.88,0.9,0.92,0.940000000000001,0.960000000000001,0.980000000000001,
0.99866513431215),.UNSPECIFIED.);
#178=B_SPLINE_CURVE_WITH_KNOTS('',5,(#21867,#21868,#21869,#21870,#21871,
#21872,#21873,#21874,#21875,#21876,#21877,#21878,#21879,#21880,#21881,#21882,
#21883,#21884,#21885,#21886,#21887,#21888,#21889,#21890,#21891,#21892,#21893,
#21894,#21895,#21896,#21897,#21898,#21899,#21900,#21901,#21902,#21903,#21904,
#21905,#21906,#21907,#21908,#21909,#21910,#21911,#21912,#21913,#21914,#21915,
#21916,#21917,#21918,#21919,#21920,#21921),.UNSPECIFIED.,.F.,.F.,(6,1,1,
1,1,1,1,1,1,1,1,1,1,1,1,1,1,1,1,1,1,1,1,1,1,1,1,1,1,1,1,1,1,1,1,1,1,1,1,
1,1,1,1,1,1,1,1,1,1,1,6),(0.,0.02,0.04,0.06,0.08,0.1,0.12,0.14,0.16,0.18,
0.2,0.22,0.24,0.26,0.28,0.3,0.32,0.34,0.36,0.38,0.4,0.42,0.44,0.46,0.48,
0.5,0.52,0.54,0.56,0.58,0.6,0.62,0.64,0.66,0.68,0.7,0.72,0.74,0.76,0.78,
0.8,0.82,0.84,0.86,0.88,0.9,0.92,0.940000000000001,0.960000000000001,0.980000000000001,
0.998665134312151),.UNSPECIFIED.);
#179=B_SPLINE_CURVE_WITH_KNOTS('',5,(#21925,#21926,#21927,#21928,#21929,
#21930,#21931,#21932,#21933,#21934,#21935,#21936,#21937,#21938,#21939,#21940,
#21941,#21942,#21943,#21944,#21945,#21946,#21947,#21948,#21949,#21950,#21951,
#21952,#21953,#21954,#21955,#21956,#21957,#21958,#21959,#21960,#21961,#21962,
#21963,#21964,#21965,#21966,#21967,#21968,#21969,#21970,#21971,#21972,#21973,
#21974,#21975,#21976,#21977,#21978,#21979),.UNSPECIFIED.,.F.,.F.,(6,1,1,
1,1,1,1,1,1,1,1,1,1,1,1,1,1,1,1,1,1,1,1,1,1,1,1,1,1,1,1,1,1,1,1,1,1,1,1,
1,1,1,1,1,1,1,1,1,1,1,6),(0.,0.02,0.04,0.06,0.08,0.1,0.12,0.14,0.16,0.18,
0.2,0.22,0.24,0.26,0.28,0.3,0.32,0.34,0.36,0.38,0.4,0.42,0.44,0.46,0.48,
0.5,0.52,0.54,0.56,0.58,0.6,0.62,0.64,0.66,0.68,0.7,0.72,0.74,0.76,0.78,
0.8,0.82,0.84,0.86,0.88,0.9,0.92,0.940000000000001,0.960000000000001,0.980000000000001,
0.99866513431215),.UNSPECIFIED.);
#180=B_SPLINE_CURVE_WITH_KNOTS('',5,(#22022,#22023,#22024,#22025,#22026,
#22027,#22028,#22029,#22030,#22031,#22032,#22033,#22034,#22035,#22036,#22037,
#22038,#22039,#22040,#22041,#22042,#22043,#22044,#22045,#22046,#22047,#22048,
#22049,#22050,#22051,#22052,#22053,#22054,#22055,#22056,#22057,#22058,#22059,
#22060,#22061,#22062,#22063,#22064,#22065,#22066,#22067,#22068,#22069,#22070,
#22071,#22072,#22073,#22074,#22075,#22076),.UNSPECIFIED.,.F.,.F.,(6,1,1,
1,1,1,1,1,1,1,1,1,1,1,1,1,1,1,1,1,1,1,1,1,1,1,1,1,1,1,1,1,1,1,1,1,1,1,1,
1,1,1,1,1,1,1,1,1,1,1,6),(0.,0.02,0.04,0.06,0.08,0.1,0.12,0.14,0.16,0.18,
0.2,0.22,0.24,0.26,0.28,0.3,0.32,0.34,0.36,0.38,0.4,0.42,0.44,0.46,0.48,
0.5,0.52,0.54,0.56,0.58,0.6,0.62,0.64,0.66,0.68,0.7,0.72,0.74,0.76,0.78,
0.8,0.82,0.84,0.86,0.88,0.9,0.92,0.940000000000001,0.960000000000001,0.980000000000001,
0.998665134312151),.UNSPECIFIED.);
#181=B_SPLINE_CURVE_WITH_KNOTS('',5,(#22255,#22256,#22257,#22258,#22259,
#22260,#22261,#22262,#22263,#22264,#22265,#22266,#22267,#22268,#22269,#22270,
#22271,#22272,#22273,#22274),.UNSPECIFIED.,.F.,.F.,(6,1,1,1,1,1,1,1,1,1,
1,1,1,1,1,6),(0.,0.0666666666666667,0.133333333333333,0.2,0.266666666666667,
0.333333333333333,0.4,0.466666666666667,0.533333333333333,0.6,0.666666666666667,
0.733333333333333,0.8,0.866666666666667,0.933333333333333,1.),
 .UNSPECIFIED.);
#182=B_SPLINE_CURVE_WITH_KNOTS('',5,(#22278,#22279,#22280,#22281,#22282,
#22283,#22284,#22285,#22286,#22287,#22288,#22289,#22290,#22291,#22292,#22293,
#22294,#22295,#22296,#22297),.UNSPECIFIED.,.F.,.F.,(6,1,1,1,1,1,1,1,1,1,
1,1,1,1,1,6),(-1.,-0.933333333333333,-0.866666666666667,-0.8,-0.733333333333333,
-0.666666666666667,-0.6,-0.533333333333333,-0.466666666666667,-0.4,-0.333333333333333,
-0.266666666666667,-0.2,-0.133333333333333,-0.0666666666666667,0.),
 .UNSPECIFIED.);
#183=B_SPLINE_CURVE_WITH_KNOTS('',3,(#22335,#22336,#22337,#22338,#22339,
#22340,#22341,#22342,#22343,#22344,#22345,#22346,#22347,#22348,#22349,#22350),
 .UNSPECIFIED.,.F.,.F.,(4,3,3,3,3,4),(0.,0.247446976985656,0.49099360586306,
0.680580226328136,0.857074929962035,0.858875452739877),.UNSPECIFIED.);
#184=B_SPLINE_CURVE_WITH_KNOTS('',3,(#22353,#22354,#22355,#22356,#22357,
#22358,#22359,#22360,#22361,#22362,#22363,#22364),.UNSPECIFIED.,.F.,.F.,
(4,2,2,2,2,4),(-0.363889062449988,-0.363126279310584,-0.288348844096792,
-0.208024613752543,-0.10483855837836,0.),.UNSPECIFIED.);
#185=B_SPLINE_CURVE_WITH_KNOTS('',5,(#22372,#22373,#22374,#22375,#22376,
#22377,#22378,#22379,#22380,#22381,#22382,#22383,#22384,#22385,#22386,#22387,
#22388,#22389,#22390,#22391),.UNSPECIFIED.,.F.,.F.,(6,1,1,1,1,1,1,1,1,1,
1,1,1,1,1,6),(0.,0.0666666666666667,0.133333333333333,0.2,0.266666666666667,
0.333333333333333,0.4,0.466666666666667,0.533333333333333,0.6,0.666666666666667,
0.733333333333333,0.8,0.866666666666667,0.933333333333333,0.989745839682859),
 .UNSPECIFIED.);
#186=B_SPLINE_CURVE_WITH_KNOTS('',3,(#22455,#22456,#22457,#22458,#22459,
#22460,#22461,#22462,#22463,#22464,#22465,#22466),.UNSPECIFIED.,.F.,.F.,
(4,2,2,2,2,4),(-0.363889062449988,-0.363126279310585,-0.288348844096793,
-0.208024613752544,-0.10483855837836,0.),.UNSPECIFIED.);
#187=B_SPLINE_CURVE_WITH_KNOTS('',3,(#22469,#22470,#22471,#22472,#22473,
#22474,#22475,#22476,#22477,#22478,#22479,#22480,#22481,#22482,#22483,#22484),
 .UNSPECIFIED.,.F.,.F.,(4,3,3,3,3,4),(0.,0.247446976985656,0.49099360586306,
0.680580226328136,0.857074929962035,0.858875452739877),.UNSPECIFIED.);
#188=B_SPLINE_CURVE_WITH_KNOTS('',5,(#22491,#22492,#22493,#22494,#22495,
#22496,#22497,#22498,#22499,#22500,#22501,#22502,#22503,#22504,#22505,#22506,
#22507,#22508,#22509,#22510),.UNSPECIFIED.,.F.,.F.,(6,1,1,1,1,1,1,1,1,1,
1,1,1,1,1,6),(0.,0.0666666666666667,0.133333333333333,0.2,0.266666666666667,
0.333333333333333,0.4,0.466666666666667,0.533333333333333,0.6,0.666666666666667,
0.733333333333333,0.8,0.866666666666667,0.933333333333333,1.),
 .UNSPECIFIED.);
#189=B_SPLINE_CURVE_WITH_KNOTS('',5,(#22561,#22562,#22563,#22564,#22565,
#22566,#22567,#22568,#22569,#22570,#22571,#22572,#22573,#22574,#22575,#22576,
#22577,#22578,#22579,#22580),.UNSPECIFIED.,.F.,.F.,(6,1,1,1,1,1,1,1,1,1,
1,1,1,1,1,6),(0.,0.0666666666666667,0.133333333333333,0.2,0.266666666666667,
0.333333333333333,0.4,0.466666666666667,0.533333333333333,0.6,0.666666666666667,
0.733333333333333,0.8,0.866666666666667,0.933333333333333,0.989745839682859),
 .UNSPECIFIED.);
#190=B_SPLINE_CURVE_WITH_KNOTS('',5,(#22605,#22606,#22607,#22608,#22609,
#22610,#22611,#22612,#22613,#22614,#22615,#22616,#22617,#22618,#22619,#22620,
#22621,#22622,#22623,#22624),.UNSPECIFIED.,.F.,.F.,(6,1,1,1,1,1,1,1,1,1,
1,1,1,1,1,6),(-1.,-0.933333333333333,-0.866666666666667,-0.8,-0.733333333333333,
-0.666666666666667,-0.6,-0.533333333333333,-0.466666666666667,-0.4,-0.333333333333333,
-0.266666666666667,-0.2,-0.133333333333333,-0.0666666666666667,0.),
 .UNSPECIFIED.);
#191=B_SPLINE_CURVE_WITH_KNOTS('',3,(#22733,#22734,#22735,#22736,#22737,
#22738,#22739,#22740,#22741,#22742,#22743,#22744,#22745,#22746,#22747,#22748,
#22749,#22750,#22751,#22752,#22753,#22754,#22755,#22756,#22757,#22758,#22759,
#22760,#22761,#22762,#22763,#22764,#22765,#22766,#22767,#22768,#22769,#22770,
#22771,#22772),.UNSPECIFIED.,.F.,.F.,(4,3,3,3,3,3,3,3,3,3,3,3,3,4),(-0.081319334915055,
-0.0753389837263114,-0.0693564459716813,-0.0633597360066557,-0.0580852392250393,
-0.0515874996582905,-0.0450649979609627,-0.0384986686708182,-0.0348511435350236,
-0.0271955520394085,-0.0193080379818354,-0.0113079400461875,-0.00319973662204704,
0.),.UNSPECIFIED.);
#192=B_SPLINE_CURVE_WITH_KNOTS('',3,(#22776,#22777,#22778,#22779,#22780,
#22781),.UNSPECIFIED.,.F.,.F.,(4,1,1,4),(0.,0.0348511435350236,0.0580852392250393,
0.081319334915055),.UNSPECIFIED.);
#193=B_SPLINE_CURVE_WITH_KNOTS('',3,(#22823,#22824,#22825,#22826,#22827,
#22828,#22829,#22830,#22831,#22832,#22833,#22834,#22835,#22836,#22837,#22838,
#22839,#22840,#22841,#22842,#22843,#22844,#22845,#22846,#22847,#22848,#22849,
#22850,#22851,#22852,#22853,#22854,#22855,#22856,#22857,#22858,#22859,#22860,
#22861,#22862),.UNSPECIFIED.,.F.,.F.,(4,3,3,3,3,3,3,3,3,3,3,3,3,4),(-0.0813193349150551,
-0.0734858773515304,-0.0657143436353313,-0.0579985436102544,-0.0504671957638769,
-0.0426591696494502,-0.0353839636779,-0.0348511435350236,-0.0290426196125197,
-0.0232340956900158,-0.016758297070707,-0.010297938217042,-0.00385507197155476,
0.),.UNSPECIFIED.);
#194=B_SPLINE_CURVE_WITH_KNOTS('',3,(#22867,#22868,#22869,#22870,#22871,
#22872),.UNSPECIFIED.,.F.,.F.,(4,1,1,4),(0.,0.0232340956900158,0.0348511435350236,
0.0813193349150551),.UNSPECIFIED.);
#195=B_SPLINE_CURVE_WITH_KNOTS('',3,(#22912,#22913,#22914,#22915,#22916,
#22917),.UNSPECIFIED.,.F.,.F.,(4,1,1,4),(-0.0804327638903581,-0.0574519742073987,
-0.0344711845244392,0.),.UNSPECIFIED.);
#196=B_SPLINE_CURVE_WITH_KNOTS('',3,(#22918,#22919,#22920,#22921,#22922,
#22923),.UNSPECIFIED.,.F.,.F.,(4,1,1,4),(0.,0.0344711845244392,0.0574519742073987,
0.0804327638903581),.UNSPECIFIED.);
#197=B_SPLINE_CURVE_WITH_KNOTS('',3,(#22958,#22959,#22960,#22961,#22962),
 .UNSPECIFIED.,.F.,.F.,(4,1,4),(-0.0804338453571326,-0.0344716480101997,
0.),.UNSPECIFIED.);
#198=B_SPLINE_CURVE_WITH_KNOTS('',3,(#22963,#22964,#22965,#22966,#22967),
 .UNSPECIFIED.,.F.,.F.,(4,1,4),(0.,0.0344716480101997,0.0804338453571326),
 .UNSPECIFIED.);
#199=B_SPLINE_CURVE_WITH_KNOTS('',3,(#22980,#22981,#22982,#22983,#22984,
#22985,#22986,#22987,#22988,#22989),.UNSPECIFIED.,.F.,.F.,(4,2,1,1,1,1,
4),(-0.00337447822145283,0.,0.176589835612662,0.353179671225324,0.529769506837986,
0.706359342450648,0.88294917806331),.UNSPECIFIED.);
#200=B_SPLINE_CURVE_WITH_KNOTS('',3,(#23066,#23067,#23068,#23069,#23070,
#23071,#23072,#23073,#23074),.UNSPECIFIED.,.F.,.F.,(4,1,1,1,1,1,4),(2.79137390763681E-5,
0.252271193732039,0.378406790598058,0.504542387464077,0.630677984330096,
0.756813581196116,0.882949178062135),.UNSPECIFIED.);
#201=B_SPLINE_CURVE_WITH_KNOTS('',3,(#23078,#23079,#23080,#23081,#23082,
#23083,#23084,#23085,#23086,#23087,#23088),.UNSPECIFIED.,.F.,.F.,(4,1,1,
1,1,1,2,4),(-0.882949178062135,-0.756813581196116,-0.630677984330096,-0.504542387464077,
-0.378406790598058,-0.252271193732039,0.,0.00337447822144074),
 .UNSPECIFIED.);
#202=B_SPLINE_CURVE_WITH_KNOTS('',3,(#23089,#23090,#23091,#23092,#23093,
#23094,#23095,#23096,#23097,#23098,#23099,#23100,#23101,#23102,#23103,#23104),
 .UNSPECIFIED.,.F.,.F.,(4,2,2,2,2,2,2,4),(-0.000760845488671771,0.,0.0228705421389603,
0.0452951187281299,0.0845262515009002,0.116879048291215,0.130924332719927,
0.145498548542211),.UNSPECIFIED.);
#203=B_SPLINE_CURVE_WITH_KNOTS('',5,(#23174,#23175,#23176,#23177,#23178,
#23179,#23180,#23181,#23182,#23183,#23184,#23185,#23186,#23187,#23188,#23189,
#23190,#23191,#23192),.UNSPECIFIED.,.F.,.F.,(6,1,1,1,1,1,1,1,1,1,1,1,1,
1,6),(-0.931895129353616,-0.866666666666667,-0.8,-0.733333333333333,-0.666666666666667,
-0.6,-0.533333333333333,-0.466666666666667,-0.4,-0.333333333333333,-0.266666666666667,
-0.2,-0.133333333333333,-0.0666666666666667,-3.17880566490557E-7),
 .UNSPECIFIED.);
#204=B_SPLINE_CURVE_WITH_KNOTS('',3,(#23197,#23198,#23199,#23200,#23201,
#23202,#23203,#23204,#23205,#23206,#23207,#23208,#23209,#23210,#23211,#23212),
 .UNSPECIFIED.,.F.,.F.,(4,2,2,2,2,2,2,4),(-0.0825251055196344,-0.08233525228657,
-0.075900251435362,-0.0686308963896873,-0.0574260404457226,-0.0407017513607544,
-0.0210184504217403,0.),.UNSPECIFIED.);
#205=B_SPLINE_CURVE_WITH_KNOTS('',3,(#23278,#23279,#23280,#23281,#23282,
#23283,#23284,#23285,#23286,#23287,#23288,#23289,#23290,#23291,#23292,#23293,
#23294,#23295,#23296,#23297,#23298,#23299,#23300,#23301,#23302,#23303,#23304,
#23305,#23306,#23307,#23308,#23309,#23310,#23311,#23312,#23313,#23314,#23315,
#23316,#23317,#23318,#23319,#23320,#23321,#23322,#23323,#23324,#23325,#23326,
#23327,#23328,#23329,#23330,#23331,#23332,#23333,#23334,#23335,#23336,#23337,
#23338,#23339,#23340,#23341,#23342,#23343,#23344,#23345,#23346,#23347,#23348,
#23349,#23350,#23351,#23352,#23353,#23354,#23355,#23356,#23357,#23358,#23359,
#23360,#23361,#23362,#23363,#23364,#23365,#23366,#23367,#23368,#23369,#23370,
#23371,#23372,#23373,#23374,#23375,#23376,#23377,#23378,#23379,#23380,#23381,
#23382,#23383,#23384,#23385,#23386,#23387,#23388,#23389,#23390,#23391,#23392,
#23393,#23394,#23395,#23396,#23397,#23398,#23399,#23400,#23401,#23402,#23403,
#23404,#23405,#23406,#23407,#23408,#23409,#23410,#23411,#23412,#23413,#23414,
#23415,#23416,#23417,#23418,#23419,#23420,#23421,#23422,#23423,#23424,#23425,
#23426,#23427,#23428,#23429,#23430,#23431,#23432,#23433,#23434),
 .UNSPECIFIED.,.F.,.F.,(4,3,3,3,3,3,3,3,3,3,3,3,3,3,3,3,3,3,3,3,3,3,3,3,
3,3,3,3,3,3,3,3,3,3,3,3,3,3,3,3,3,3,3,3,3,3,3,3,3,3,3,3,4),(-4.43919555064984,
-4.31351752310522,-4.21748497989632,-4.13039569871212,-4.04917309818115,
-3.97216182461211,-3.89780976908328,-3.82536061976307,-3.75520238328067,
-3.68765512117113,-3.62163278915582,-3.55440616562861,-3.48496721361178,
-3.40927574040849,-3.3121488002462,-3.22434990344501,-3.15109446525443,
-3.08492269429087,-3.02341966724156,-2.96461369321188,-2.90551252744871,
-2.84539597265316,-2.78402646194644,-2.72077433031378,-2.65518089902205,
-2.58678643782235,-2.51494173113323,-2.4351726591892,-2.3469342569877,-2.24741963324518,
-2.1576576071755,-2.0742009601071,-1.99319641369387,-1.91148636863784,-1.82737832465568,
-1.74166088715984,-1.65491799562197,-1.56650259700221,-1.4759044479693,
-1.3822422658407,-1.28644440225838,-1.18824460058421,-1.087792421038,-0.985316046032208,
-0.877949096049762,-0.75542711973491,-0.615520892462394,-0.46127383549543,
-0.336504337401264,-0.222259848570182,-0.111129924285091,-0.0120794939036124,
0.),.UNSPECIFIED.);
#206=B_SPLINE_CURVE_WITH_KNOTS('',5,(#23512,#23513,#23514,#23515,#23516,
#23517,#23518,#23519,#23520,#23521,#23522,#23523,#23524,#23525,#23526,#23527,
#23528,#23529,#23530,#23531,#23532,#23533,#23534,#23535,#23536,#23537,#23538,
#23539,#23540,#23541,#23542,#23543,#23544),.UNSPECIFIED.,.F.,.F.,(6,1,1,
1,1,1,1,1,1,1,1,1,1,1,1,1,1,1,1,1,1,1,1,1,1,1,1,1,6),(-0.998665134312148,
-0.980000000000001,-0.960000000000001,-0.940000000000001,-0.92,-0.9,-0.88,
-0.86,-0.84,-0.82,-0.8,-0.78,-0.76,-0.74,-0.72,-0.7,-0.68,-0.66,-0.64,-0.62,
-0.6,-0.58,-0.56,-0.54,-0.52,-0.5,-0.48,-0.46,-0.45747490134806),
 .UNSPECIFIED.);
#207=ELLIPSE('',#4296,1.6218841056004,1.5);
#208=ELLIPSE('',#4297,1.6218841056004,1.5);
#209=ELLIPSE('',#4366,1.6218841056004,1.5);
#210=ELLIPSE('',#4367,1.6218841056004,1.5);
#211=ELLIPSE('',#4610,0.440642274355316,0.384283137019794);
#212=ELLIPSE('',#4613,0.440642274355316,0.384283137019794);
#213=TOROIDAL_SURFACE('',#4285,1.70133516896762,0.5);
#214=TOROIDAL_SURFACE('',#4290,1.75974879114541,0.5);
#215=TOROIDAL_SURFACE('',#4355,1.70133516896762,0.5);
#216=TOROIDAL_SURFACE('',#4360,1.75974879114541,0.5);
#217=TOROIDAL_SURFACE('',#4486,63.3332952479771,1.);
#218=TOROIDAL_SURFACE('',#4490,50.7730300598816,1.);
#219=TOROIDAL_SURFACE('',#4500,63.3332952479771,1.);
#220=TOROIDAL_SURFACE('',#4503,50.7730300598816,1.);
#221=TOROIDAL_SURFACE('',#4513,1.49422838778107,0.75);
#222=TOROIDAL_SURFACE('',#4519,1.48767572173512,0.75);
#223=TOROIDAL_SURFACE('',#4525,1.49422838778107,0.75);
#224=TOROIDAL_SURFACE('',#4532,1.48767572173512,0.75);
#225=TOROIDAL_SURFACE('',#4625,62.8868723549169,1.);
#226=TOROIDAL_SURFACE('',#4630,62.8868723549169,1.);
#227=TOROIDAL_SURFACE('',#4638,18.7866355153418,1.);
#228=TOROIDAL_SURFACE('',#4647,18.7866355153418,1.);
#229=SHAPE_REPRESENTATION_RELATIONSHIP('SRR','None',#23612,#238);
#230=SHAPE_REPRESENTATION_RELATIONSHIP('SRR','None',#23613,#239);
#231=SHAPE_REPRESENTATION_RELATIONSHIP('SRR','None',#23614,#240);
#232=SHAPE_REPRESENTATION_RELATIONSHIP('SRR','None',#23615,#241);
#233=SHAPE_REPRESENTATION_RELATIONSHIP('SRR','None',#23616,#242);
#234=SHAPE_REPRESENTATION_RELATIONSHIP('SRR','None',#23617,#243);
#235=SHAPE_REPRESENTATION_RELATIONSHIP('SRR','None',#23618,#244);
#236=SHAPE_REPRESENTATION_RELATIONSHIP('SRR','None',#23619,#245);
#237=SHAPE_REPRESENTATION_RELATIONSHIP('SRR','None',#23620,#246);
#238=ADVANCED_BREP_SHAPE_REPRESENTATION('',(#256),#23568);
#239=ADVANCED_BREP_SHAPE_REPRESENTATION('',(#257),#23569);
#240=ADVANCED_BREP_SHAPE_REPRESENTATION('',(#258),#23570);
#241=ADVANCED_BREP_SHAPE_REPRESENTATION('',(#259),#23571);
#242=ADVANCED_BREP_SHAPE_REPRESENTATION('',(#260),#23572);
#243=ADVANCED_BREP_SHAPE_REPRESENTATION('',(#261),#23573);
#244=ADVANCED_BREP_SHAPE_REPRESENTATION('',(#262),#23574);
#245=ADVANCED_BREP_SHAPE_REPRESENTATION('',(#263),#23575);
#246=ADVANCED_BREP_SHAPE_REPRESENTATION('',(#264),#23576);
#247=STYLED_ITEM('',(#23666),#256);
#248=STYLED_ITEM('',(#23666),#257);
#249=STYLED_ITEM('',(#23666),#258);
#250=STYLED_ITEM('',(#23666),#259);
#251=STYLED_ITEM('',(#23667),#260);
#252=STYLED_ITEM('',(#23666),#261);
#253=STYLED_ITEM('',(#23668),#262);
#254=STYLED_ITEM('',(#23666),#263);
#255=STYLED_ITEM('',(#23669),#264);
#256=MANIFOLD_SOLID_BREP('Body1',#4157);
#257=MANIFOLD_SOLID_BREP('Body1',#4158);
#258=MANIFOLD_SOLID_BREP('Body1',#4159);
#259=MANIFOLD_SOLID_BREP('Body1',#4160);
#260=MANIFOLD_SOLID_BREP('Body1',#4161);
#261=MANIFOLD_SOLID_BREP('Body1',#4162);
#262=MANIFOLD_SOLID_BREP('Body1',#4163);
#263=MANIFOLD_SOLID_BREP('Body1',#4164);
#264=MANIFOLD_SOLID_BREP('Body1',#4165);
#265=FACE_BOUND('',#629,.T.);
#266=FACE_BOUND('',#630,.T.);
#267=FACE_BOUND('',#632,.T.);
#268=FACE_BOUND('',#633,.T.);
#269=FACE_BOUND('',#640,.T.);
#270=FACE_BOUND('',#641,.T.);
#271=FACE_BOUND('',#670,.T.);
#272=FACE_BOUND('',#671,.T.);
#273=FACE_BOUND('',#673,.T.);
#274=FACE_BOUND('',#674,.T.);
#275=FACE_BOUND('',#681,.T.);
#276=FACE_BOUND('',#682,.T.);
#277=FACE_BOUND('',#686,.T.);
#278=FACE_BOUND('',#687,.T.);
#279=FACE_BOUND('',#714,.T.);
#280=FACE_BOUND('',#715,.T.);
#281=FACE_BOUND('',#724,.T.);
#282=FACE_BOUND('',#726,.T.);
#283=FACE_BOUND('',#755,.T.);
#284=FACE_BOUND('',#767,.T.);
#285=FACE_BOUND('',#769,.T.);
#286=FACE_BOUND('',#778,.T.);
#287=FACE_BOUND('',#779,.T.);
#288=FACE_BOUND('',#800,.T.);
#289=FACE_BOUND('',#801,.T.);
#290=FACE_BOUND('',#803,.T.);
#291=FACE_BOUND('',#804,.T.);
#292=FACE_BOUND('',#809,.T.);
#293=FACE_BOUND('',#810,.T.);
#294=FACE_BOUND('',#822,.T.);
#295=FACE_BOUND('',#823,.T.);
#296=FACE_BOUND('',#829,.T.);
#297=FACE_BOUND('',#836,.T.);
#298=FACE_BOUND('',#842,.T.);
#299=FACE_BOUND('',#843,.T.);
#300=PLANE('',#4277);
#301=PLANE('',#4281);
#302=PLANE('',#4282);
#303=PLANE('',#4283);
#304=PLANE('',#4289);
#305=PLANE('',#4294);
#306=PLANE('',#4298);
#307=PLANE('',#4308);
#308=PLANE('',#4311);
#309=PLANE('',#4314);
#310=PLANE('',#4317);
#311=PLANE('',#4320);
#312=PLANE('',#4325);
#313=PLANE('',#4326);
#314=PLANE('',#4327);
#315=PLANE('',#4328);
#316=PLANE('',#4332);
#317=PLANE('',#4336);
#318=PLANE('',#4340);
#319=PLANE('',#4344);
#320=PLANE('',#4348);
#321=PLANE('',#4352);
#322=PLANE('',#4353);
#323=PLANE('',#4359);
#324=PLANE('',#4364);
#325=PLANE('',#4368);
#326=PLANE('',#4378);
#327=PLANE('',#4379);
#328=PLANE('',#4388);
#329=PLANE('',#4391);
#330=PLANE('',#4394);
#331=PLANE('',#4397);
#332=PLANE('',#4402);
#333=PLANE('',#4403);
#334=PLANE('',#4404);
#335=PLANE('',#4405);
#336=PLANE('',#4408);
#337=PLANE('',#4411);
#338=PLANE('',#4414);
#339=PLANE('',#4417);
#340=PLANE('',#4420);
#341=PLANE('',#4423);
#342=PLANE('',#4428);
#343=PLANE('',#4429);
#344=PLANE('',#4430);
#345=PLANE('',#4431);
#346=PLANE('',#4432);
#347=PLANE('',#4433);
#348=PLANE('',#4434);
#349=PLANE('',#4435);
#350=PLANE('',#4465);
#351=PLANE('',#4466);
#352=PLANE('',#4472);
#353=PLANE('',#4477);
#354=PLANE('',#4478);
#355=PLANE('',#4479);
#356=PLANE('',#4480);
#357=PLANE('',#4481);
#358=PLANE('',#4482);
#359=PLANE('',#4483);
#360=PLANE('',#4484);
#361=PLANE('',#4505);
#362=PLANE('',#4511);
#363=PLANE('',#4516);
#364=PLANE('',#4517);
#365=PLANE('',#4522);
#366=PLANE('',#4523);
#367=PLANE('',#4529);
#368=PLANE('',#4530);
#369=PLANE('',#4536);
#370=PLANE('',#4541);
#371=PLANE('',#4551);
#372=PLANE('',#4552);
#373=PLANE('',#4555);
#374=PLANE('',#4560);
#375=PLANE('',#4568);
#376=PLANE('',#4569);
#377=PLANE('',#4574);
#378=PLANE('',#4580);
#379=PLANE('',#4581);
#380=PLANE('',#4582);
#381=PLANE('',#4583);
#382=PLANE('',#4586);
#383=PLANE('',#4593);
#384=PLANE('',#4600);
#385=PLANE('',#4601);
#386=PLANE('',#4602);
#387=PLANE('',#4605);
#388=PLANE('',#4606);
#389=PLANE('',#4622);
#390=PLANE('',#4633);
#391=PLANE('',#4646);
#392=PLANE('',#4657);
#393=PLANE('',#4658);
#394=PLANE('',#4662);
#395=PLANE('',#4663);
#396=FACE_OUTER_BOUND('',#622,.T.);
#397=FACE_OUTER_BOUND('',#623,.T.);
#398=FACE_OUTER_BOUND('',#624,.T.);
#399=FACE_OUTER_BOUND('',#625,.T.);
#400=FACE_OUTER_BOUND('',#626,.T.);
#401=FACE_OUTER_BOUND('',#627,.T.);
#402=FACE_OUTER_BOUND('',#628,.T.);
#403=FACE_OUTER_BOUND('',#631,.T.);
#404=FACE_OUTER_BOUND('',#634,.T.);
#405=FACE_OUTER_BOUND('',#635,.T.);
#406=FACE_OUTER_BOUND('',#636,.T.);
#407=FACE_OUTER_BOUND('',#637,.T.);
#408=FACE_OUTER_BOUND('',#638,.T.);
#409=FACE_OUTER_BOUND('',#639,.T.);
#410=FACE_OUTER_BOUND('',#642,.T.);
#411=FACE_OUTER_BOUND('',#643,.T.);
#412=FACE_OUTER_BOUND('',#644,.T.);
#413=FACE_OUTER_BOUND('',#645,.T.);
#414=FACE_OUTER_BOUND('',#646,.T.);
#415=FACE_OUTER_BOUND('',#647,.T.);
#416=FACE_OUTER_BOUND('',#648,.T.);
#417=FACE_OUTER_BOUND('',#649,.T.);
#418=FACE_OUTER_BOUND('',#650,.T.);
#419=FACE_OUTER_BOUND('',#651,.T.);
#420=FACE_OUTER_BOUND('',#652,.T.);
#421=FACE_OUTER_BOUND('',#653,.T.);
#422=FACE_OUTER_BOUND('',#654,.T.);
#423=FACE_OUTER_BOUND('',#655,.T.);
#424=FACE_OUTER_BOUND('',#656,.T.);
#425=FACE_OUTER_BOUND('',#657,.T.);
#426=FACE_OUTER_BOUND('',#658,.T.);
#427=FACE_OUTER_BOUND('',#659,.T.);
#428=FACE_OUTER_BOUND('',#660,.T.);
#429=FACE_OUTER_BOUND('',#661,.T.);
#430=FACE_OUTER_BOUND('',#662,.T.);
#431=FACE_OUTER_BOUND('',#663,.T.);
#432=FACE_OUTER_BOUND('',#664,.T.);
#433=FACE_OUTER_BOUND('',#665,.T.);
#434=FACE_OUTER_BOUND('',#666,.T.);
#435=FACE_OUTER_BOUND('',#667,.T.);
#436=FACE_OUTER_BOUND('',#668,.T.);
#437=FACE_OUTER_BOUND('',#669,.T.);
#438=FACE_OUTER_BOUND('',#672,.T.);
#439=FACE_OUTER_BOUND('',#675,.T.);
#440=FACE_OUTER_BOUND('',#676,.T.);
#441=FACE_OUTER_BOUND('',#677,.T.);
#442=FACE_OUTER_BOUND('',#678,.T.);
#443=FACE_OUTER_BOUND('',#679,.T.);
#444=FACE_OUTER_BOUND('',#680,.T.);
#445=FACE_OUTER_BOUND('',#683,.T.);
#446=FACE_OUTER_BOUND('',#684,.T.);
#447=FACE_OUTER_BOUND('',#685,.T.);
#448=FACE_OUTER_BOUND('',#688,.T.);
#449=FACE_OUTER_BOUND('',#689,.T.);
#450=FACE_OUTER_BOUND('',#690,.T.);
#451=FACE_OUTER_BOUND('',#691,.T.);
#452=FACE_OUTER_BOUND('',#692,.T.);
#453=FACE_OUTER_BOUND('',#693,.T.);
#454=FACE_OUTER_BOUND('',#694,.T.);
#455=FACE_OUTER_BOUND('',#695,.T.);
#456=FACE_OUTER_BOUND('',#696,.T.);
#457=FACE_OUTER_BOUND('',#697,.T.);
#458=FACE_OUTER_BOUND('',#698,.T.);
#459=FACE_OUTER_BOUND('',#699,.T.);
#460=FACE_OUTER_BOUND('',#700,.T.);
#461=FACE_OUTER_BOUND('',#701,.T.);
#462=FACE_OUTER_BOUND('',#702,.T.);
#463=FACE_OUTER_BOUND('',#703,.T.);
#464=FACE_OUTER_BOUND('',#704,.T.);
#465=FACE_OUTER_BOUND('',#705,.T.);
#466=FACE_OUTER_BOUND('',#706,.T.);
#467=FACE_OUTER_BOUND('',#707,.T.);
#468=FACE_OUTER_BOUND('',#708,.T.);
#469=FACE_OUTER_BOUND('',#709,.T.);
#470=FACE_OUTER_BOUND('',#710,.T.);
#471=FACE_OUTER_BOUND('',#711,.T.);
#472=FACE_OUTER_BOUND('',#712,.T.);
#473=FACE_OUTER_BOUND('',#713,.T.);
#474=FACE_OUTER_BOUND('',#716,.T.);
#475=FACE_OUTER_BOUND('',#717,.T.);
#476=FACE_OUTER_BOUND('',#718,.T.);
#477=FACE_OUTER_BOUND('',#719,.T.);
#478=FACE_OUTER_BOUND('',#720,.T.);
#479=FACE_OUTER_BOUND('',#721,.T.);
#480=FACE_OUTER_BOUND('',#722,.T.);
#481=FACE_OUTER_BOUND('',#723,.T.);
#482=FACE_OUTER_BOUND('',#725,.T.);
#483=FACE_OUTER_BOUND('',#727,.T.);
#484=FACE_OUTER_BOUND('',#728,.T.);
#485=FACE_OUTER_BOUND('',#729,.T.);
#486=FACE_OUTER_BOUND('',#730,.T.);
#487=FACE_OUTER_BOUND('',#731,.T.);
#488=FACE_OUTER_BOUND('',#732,.T.);
#489=FACE_OUTER_BOUND('',#733,.T.);
#490=FACE_OUTER_BOUND('',#734,.T.);
#491=FACE_OUTER_BOUND('',#735,.T.);
#492=FACE_OUTER_BOUND('',#736,.T.);
#493=FACE_OUTER_BOUND('',#737,.T.);
#494=FACE_OUTER_BOUND('',#738,.T.);
#495=FACE_OUTER_BOUND('',#739,.T.);
#496=FACE_OUTER_BOUND('',#740,.T.);
#497=FACE_OUTER_BOUND('',#741,.T.);
#498=FACE_OUTER_BOUND('',#742,.T.);
#499=FACE_OUTER_BOUND('',#743,.T.);
#500=FACE_OUTER_BOUND('',#744,.T.);
#501=FACE_OUTER_BOUND('',#745,.T.);
#502=FACE_OUTER_BOUND('',#746,.T.);
#503=FACE_OUTER_BOUND('',#747,.T.);
#504=FACE_OUTER_BOUND('',#748,.T.);
#505=FACE_OUTER_BOUND('',#749,.T.);
#506=FACE_OUTER_BOUND('',#750,.T.);
#507=FACE_OUTER_BOUND('',#751,.T.);
#508=FACE_OUTER_BOUND('',#752,.T.);
#509=FACE_OUTER_BOUND('',#753,.T.);
#510=FACE_OUTER_BOUND('',#754,.T.);
#511=FACE_OUTER_BOUND('',#756,.T.);
#512=FACE_OUTER_BOUND('',#757,.T.);
#513=FACE_OUTER_BOUND('',#758,.T.);
#514=FACE_OUTER_BOUND('',#759,.T.);
#515=FACE_OUTER_BOUND('',#760,.T.);
#516=FACE_OUTER_BOUND('',#761,.T.);
#517=FACE_OUTER_BOUND('',#762,.T.);
#518=FACE_OUTER_BOUND('',#763,.T.);
#519=FACE_OUTER_BOUND('',#764,.T.);
#520=FACE_OUTER_BOUND('',#765,.T.);
#521=FACE_OUTER_BOUND('',#766,.T.);
#522=FACE_OUTER_BOUND('',#768,.T.);
#523=FACE_OUTER_BOUND('',#770,.T.);
#524=FACE_OUTER_BOUND('',#771,.T.);
#525=FACE_OUTER_BOUND('',#772,.T.);
#526=FACE_OUTER_BOUND('',#773,.T.);
#527=FACE_OUTER_BOUND('',#774,.T.);
#528=FACE_OUTER_BOUND('',#775,.T.);
#529=FACE_OUTER_BOUND('',#776,.T.);
#530=FACE_OUTER_BOUND('',#777,.T.);
#531=FACE_OUTER_BOUND('',#780,.T.);
#532=FACE_OUTER_BOUND('',#781,.T.);
#533=FACE_OUTER_BOUND('',#782,.T.);
#534=FACE_OUTER_BOUND('',#783,.T.);
#535=FACE_OUTER_BOUND('',#784,.T.);
#536=FACE_OUTER_BOUND('',#785,.T.);
#537=FACE_OUTER_BOUND('',#786,.T.);
#538=FACE_OUTER_BOUND('',#787,.T.);
#539=FACE_OUTER_BOUND('',#788,.T.);
#540=FACE_OUTER_BOUND('',#789,.T.);
#541=FACE_OUTER_BOUND('',#790,.T.);
#542=FACE_OUTER_BOUND('',#791,.T.);
#543=FACE_OUTER_BOUND('',#792,.T.);
#544=FACE_OUTER_BOUND('',#793,.T.);
#545=FACE_OUTER_BOUND('',#794,.T.);
#546=FACE_OUTER_BOUND('',#795,.T.);
#547=FACE_OUTER_BOUND('',#796,.T.);
#548=FACE_OUTER_BOUND('',#797,.T.);
#549=FACE_OUTER_BOUND('',#798,.T.);
#550=FACE_OUTER_BOUND('',#799,.T.);
#551=FACE_OUTER_BOUND('',#802,.T.);
#552=FACE_OUTER_BOUND('',#805,.T.);
#553=FACE_OUTER_BOUND('',#806,.T.);
#554=FACE_OUTER_BOUND('',#807,.T.);
#555=FACE_OUTER_BOUND('',#808,.T.);
#556=FACE_OUTER_BOUND('',#811,.T.);
#557=FACE_OUTER_BOUND('',#812,.T.);
#558=FACE_OUTER_BOUND('',#813,.T.);
#559=FACE_OUTER_BOUND('',#814,.T.);
#560=FACE_OUTER_BOUND('',#815,.T.);
#561=FACE_OUTER_BOUND('',#816,.T.);
#562=FACE_OUTER_BOUND('',#817,.T.);
#563=FACE_OUTER_BOUND('',#818,.T.);
#564=FACE_OUTER_BOUND('',#819,.T.);
#565=FACE_OUTER_BOUND('',#820,.T.);
#566=FACE_OUTER_BOUND('',#821,.T.);
#567=FACE_OUTER_BOUND('',#824,.T.);
#568=FACE_OUTER_BOUND('',#825,.T.);
#569=FACE_OUTER_BOUND('',#826,.T.);
#570=FACE_OUTER_BOUND('',#827,.T.);
#571=FACE_OUTER_BOUND('',#828,.T.);
#572=FACE_OUTER_BOUND('',#830,.T.);
#573=FACE_OUTER_BOUND('',#831,.T.);
#574=FACE_OUTER_BOUND('',#832,.T.);
#575=FACE_OUTER_BOUND('',#833,.T.);
#576=FACE_OUTER_BOUND('',#834,.T.);
#577=FACE_OUTER_BOUND('',#835,.T.);
#578=FACE_OUTER_BOUND('',#837,.T.);
#579=FACE_OUTER_BOUND('',#838,.T.);
#580=FACE_OUTER_BOUND('',#839,.T.);
#581=FACE_OUTER_BOUND('',#840,.T.);
#582=FACE_OUTER_BOUND('',#841,.T.);
#583=FACE_OUTER_BOUND('',#844,.T.);
#584=FACE_OUTER_BOUND('',#845,.T.);
#585=FACE_OUTER_BOUND('',#846,.T.);
#586=FACE_OUTER_BOUND('',#847,.T.);
#587=FACE_OUTER_BOUND('',#848,.T.);
#588=FACE_OUTER_BOUND('',#849,.T.);
#589=FACE_OUTER_BOUND('',#850,.T.);
#590=FACE_OUTER_BOUND('',#851,.T.);
#591=FACE_OUTER_BOUND('',#852,.T.);
#592=FACE_OUTER_BOUND('',#853,.T.);
#593=FACE_OUTER_BOUND('',#854,.T.);
#594=FACE_OUTER_BOUND('',#855,.T.);
#595=FACE_OUTER_BOUND('',#856,.T.);
#596=FACE_OUTER_BOUND('',#857,.T.);
#597=FACE_OUTER_BOUND('',#858,.T.);
#598=FACE_OUTER_BOUND('',#859,.T.);
#599=FACE_OUTER_BOUND('',#860,.T.);
#600=FACE_OUTER_BOUND('',#861,.T.);
#601=FACE_OUTER_BOUND('',#862,.T.);
#602=FACE_OUTER_BOUND('',#863,.T.);
#603=FACE_OUTER_BOUND('',#864,.T.);
#604=FACE_OUTER_BOUND('',#865,.T.);
#605=FACE_OUTER_BOUND('',#866,.T.);
#606=FACE_OUTER_BOUND('',#867,.T.);
#607=FACE_OUTER_BOUND('',#868,.T.);
#608=FACE_OUTER_BOUND('',#869,.T.);
#609=FACE_OUTER_BOUND('',#870,.T.);
#610=FACE_OUTER_BOUND('',#871,.T.);
#611=FACE_OUTER_BOUND('',#872,.T.);
#612=FACE_OUTER_BOUND('',#873,.T.);
#613=FACE_OUTER_BOUND('',#874,.T.);
#614=FACE_OUTER_BOUND('',#875,.T.);
#615=FACE_OUTER_BOUND('',#876,.T.);
#616=FACE_OUTER_BOUND('',#877,.T.);
#617=FACE_OUTER_BOUND('',#878,.T.);
#618=FACE_OUTER_BOUND('',#879,.T.);
#619=FACE_OUTER_BOUND('',#880,.T.);
#620=FACE_OUTER_BOUND('',#881,.T.);
#621=FACE_OUTER_BOUND('',#882,.T.);
#622=EDGE_LOOP('',(#2637,#2638,#2639,#2640));
#623=EDGE_LOOP('',(#2641,#2642,#2643,#2644));
#624=EDGE_LOOP('',(#2645,#2646,#2647,#2648));
#625=EDGE_LOOP('',(#2649,#2650,#2651,#2652));
#626=EDGE_LOOP('',(#2653,#2654,#2655,#2656));
#627=EDGE_LOOP('',(#2657,#2658,#2659,#2660));
#628=EDGE_LOOP('',(#2661,#2662,#2663,#2664));
#629=EDGE_LOOP('',(#2665));
#630=EDGE_LOOP('',(#2666));
#631=EDGE_LOOP('',(#2667,#2668,#2669,#2670));
#632=EDGE_LOOP('',(#2671));
#633=EDGE_LOOP('',(#2672));
#634=EDGE_LOOP('',(#2673,#2674,#2675,#2676));
#635=EDGE_LOOP('',(#2677));
#636=EDGE_LOOP('',(#2678,#2679,#2680,#2681));
#637=EDGE_LOOP('',(#2682));
#638=EDGE_LOOP('',(#2683,#2684,#2685,#2686));
#639=EDGE_LOOP('',(#2687,#2688,#2689,#2690,#2691,#2692,#2693,#2694,#2695,
#2696,#2697,#2698,#2699,#2700));
#640=EDGE_LOOP('',(#2701));
#641=EDGE_LOOP('',(#2702));
#642=EDGE_LOOP('',(#2703,#2704,#2705,#2706));
#643=EDGE_LOOP('',(#2707,#2708,#2709,#2710));
#644=EDGE_LOOP('',(#2711,#2712,#2713,#2714));
#645=EDGE_LOOP('',(#2715,#2716,#2717,#2718));
#646=EDGE_LOOP('',(#2719,#2720,#2721,#2722));
#647=EDGE_LOOP('',(#2723,#2724,#2725,#2726,#2727));
#648=EDGE_LOOP('',(#2728,#2729,#2730,#2731));
#649=EDGE_LOOP('',(#2732,#2733,#2734,#2735,#2736));
#650=EDGE_LOOP('',(#2737,#2738,#2739,#2740));
#651=EDGE_LOOP('',(#2741,#2742,#2743,#2744));
#652=EDGE_LOOP('',(#2745,#2746,#2747,#2748));
#653=EDGE_LOOP('',(#2749,#2750,#2751,#2752));
#654=EDGE_LOOP('',(#2753,#2754,#2755,#2756,#2757));
#655=EDGE_LOOP('',(#2758,#2759,#2760,#2761,#2762,#2763,#2764,#2765,#2766,
#2767,#2768,#2769,#2770,#2771,#2772,#2773));
#656=EDGE_LOOP('',(#2774,#2775,#2776,#2777));
#657=EDGE_LOOP('',(#2778,#2779,#2780,#2781));
#658=EDGE_LOOP('',(#2782,#2783,#2784,#2785));
#659=EDGE_LOOP('',(#2786,#2787,#2788,#2789));
#660=EDGE_LOOP('',(#2790,#2791,#2792,#2793));
#661=EDGE_LOOP('',(#2794,#2795,#2796,#2797));
#662=EDGE_LOOP('',(#2798,#2799,#2800,#2801));
#663=EDGE_LOOP('',(#2802,#2803,#2804,#2805));
#664=EDGE_LOOP('',(#2806,#2807,#2808,#2809));
#665=EDGE_LOOP('',(#2810,#2811,#2812,#2813,#2814));
#666=EDGE_LOOP('',(#2815,#2816,#2817,#2818));
#667=EDGE_LOOP('',(#2819,#2820,#2821,#2822));
#668=EDGE_LOOP('',(#2823,#2824,#2825,#2826));
#669=EDGE_LOOP('',(#2827,#2828,#2829,#2830,#2831,#2832));
#670=EDGE_LOOP('',(#2833,#2834,#2835,#2836));
#671=EDGE_LOOP('',(#2837,#2838,#2839,#2840));
#672=EDGE_LOOP('',(#2841,#2842,#2843,#2844,#2845,#2846));
#673=EDGE_LOOP('',(#2847,#2848,#2849,#2850));
#674=EDGE_LOOP('',(#2851,#2852,#2853,#2854));
#675=EDGE_LOOP('',(#2855,#2856,#2857,#2858));
#676=EDGE_LOOP('',(#2859));
#677=EDGE_LOOP('',(#2860,#2861,#2862,#2863));
#678=EDGE_LOOP('',(#2864));
#679=EDGE_LOOP('',(#2865,#2866,#2867,#2868));
#680=EDGE_LOOP('',(#2869,#2870,#2871,#2872,#2873,#2874));
#681=EDGE_LOOP('',(#2875,#2876,#2877,#2878));
#682=EDGE_LOOP('',(#2879,#2880,#2881,#2882));
#683=EDGE_LOOP('',(#2883,#2884,#2885,#2886));
#684=EDGE_LOOP('',(#2887,#2888,#2889,#2890));
#685=EDGE_LOOP('',(#2891,#2892,#2893,#2894,#2895,#2896,#2897,#2898,#2899,
#2900,#2901,#2902,#2903,#2904));
#686=EDGE_LOOP('',(#2905));
#687=EDGE_LOOP('',(#2906));
#688=EDGE_LOOP('',(#2907,#2908,#2909,#2910));
#689=EDGE_LOOP('',(#2911,#2912,#2913,#2914));
#690=EDGE_LOOP('',(#2915,#2916,#2917,#2918));
#691=EDGE_LOOP('',(#2919,#2920,#2921,#2922,#2923));
#692=EDGE_LOOP('',(#2924,#2925,#2926,#2927));
#693=EDGE_LOOP('',(#2928,#2929,#2930,#2931,#2932));
#694=EDGE_LOOP('',(#2933,#2934,#2935,#2936));
#695=EDGE_LOOP('',(#2937,#2938,#2939,#2940));
#696=EDGE_LOOP('',(#2941,#2942,#2943,#2944));
#697=EDGE_LOOP('',(#2945,#2946,#2947,#2948));
#698=EDGE_LOOP('',(#2949,#2950,#2951,#2952,#2953));
#699=EDGE_LOOP('',(#2954,#2955,#2956,#2957,#2958,#2959,#2960,#2961,#2962,
#2963,#2964,#2965,#2966,#2967,#2968,#2969));
#700=EDGE_LOOP('',(#2970,#2971,#2972,#2973));
#701=EDGE_LOOP('',(#2974,#2975,#2976,#2977));
#702=EDGE_LOOP('',(#2978,#2979,#2980,#2981));
#703=EDGE_LOOP('',(#2982,#2983,#2984,#2985));
#704=EDGE_LOOP('',(#2986,#2987,#2988,#2989));
#705=EDGE_LOOP('',(#2990,#2991,#2992,#2993));
#706=EDGE_LOOP('',(#2994,#2995,#2996,#2997));
#707=EDGE_LOOP('',(#2998,#2999,#3000,#3001));
#708=EDGE_LOOP('',(#3002,#3003,#3004,#3005));
#709=EDGE_LOOP('',(#3006,#3007,#3008,#3009,#3010));
#710=EDGE_LOOP('',(#3011,#3012,#3013,#3014));
#711=EDGE_LOOP('',(#3015,#3016,#3017,#3018));
#712=EDGE_LOOP('',(#3019,#3020,#3021,#3022));
#713=EDGE_LOOP('',(#3023,#3024,#3025,#3026,#3027,#3028));
#714=EDGE_LOOP('',(#3029,#3030,#3031,#3032));
#715=EDGE_LOOP('',(#3033,#3034,#3035,#3036));
#716=EDGE_LOOP('',(#3037,#3038,#3039,#3040));
#717=EDGE_LOOP('',(#3041,#3042,#3043,#3044));
#718=EDGE_LOOP('',(#3045,#3046,#3047,#3048));
#719=EDGE_LOOP('',(#3049,#3050,#3051,#3052));
#720=EDGE_LOOP('',(#3053,#3054,#3055,#3056));
#721=EDGE_LOOP('',(#3057,#3058,#3059,#3060));
#722=EDGE_LOOP('',(#3061,#3062,#3063,#3064));
#723=EDGE_LOOP('',(#3065,#3066,#3067,#3068,#3069,#3070));
#724=EDGE_LOOP('',(#3071));
#725=EDGE_LOOP('',(#3072,#3073,#3074,#3075,#3076,#3077));
#726=EDGE_LOOP('',(#3078));
#727=EDGE_LOOP('',(#3079,#3080,#3081,#3082));
#728=EDGE_LOOP('',(#3083,#3084,#3085,#3086));
#729=EDGE_LOOP('',(#3087,#3088,#3089,#3090));
#730=EDGE_LOOP('',(#3091,#3092,#3093,#3094));
#731=EDGE_LOOP('',(#3095,#3096,#3097,#3098));
#732=EDGE_LOOP('',(#3099,#3100,#3101,#3102));
#733=EDGE_LOOP('',(#3103,#3104,#3105,#3106));
#734=EDGE_LOOP('',(#3107,#3108,#3109,#3110));
#735=EDGE_LOOP('',(#3111,#3112,#3113,#3114));
#736=EDGE_LOOP('',(#3115,#3116,#3117,#3118));
#737=EDGE_LOOP('',(#3119,#3120,#3121,#3122,#3123));
#738=EDGE_LOOP('',(#3124,#3125,#3126,#3127));
#739=EDGE_LOOP('',(#3128,#3129,#3130,#3131,#3132));
#740=EDGE_LOOP('',(#3133,#3134,#3135,#3136));
#741=EDGE_LOOP('',(#3137,#3138,#3139,#3140));
#742=EDGE_LOOP('',(#3141,#3142,#3143,#3144));
#743=EDGE_LOOP('',(#3145,#3146,#3147,#3148));
#744=EDGE_LOOP('',(#3149,#3150,#3151,#3152));
#745=EDGE_LOOP('',(#3153,#3154,#3155,#3156));
#746=EDGE_LOOP('',(#3157,#3158,#3159,#3160));
#747=EDGE_LOOP('',(#3161,#3162,#3163,#3164));
#748=EDGE_LOOP('',(#3165,#3166,#3167,#3168));
#749=EDGE_LOOP('',(#3169,#3170,#3171,#3172,#3173,#3174,#3175,#3176,#3177,
#3178,#3179,#3180,#3181,#3182,#3183,#3184,#3185,#3186,#3187,#3188,#3189,
#3190,#3191,#3192,#3193,#3194,#3195,#3196,#3197,#3198,#3199,#3200,#3201,
#3202,#3203,#3204,#3205,#3206,#3207,#3208,#3209,#3210,#3211,#3212,#3213,
#3214,#3215,#3216,#3217,#3218));
#750=EDGE_LOOP('',(#3219,#3220,#3221,#3222));
#751=EDGE_LOOP('',(#3223,#3224,#3225,#3226,#3227,#3228,#3229,#3230,#3231,
#3232,#3233,#3234,#3235,#3236,#3237,#3238,#3239,#3240,#3241,#3242,#3243,
#3244,#3245,#3246,#3247,#3248,#3249,#3250,#3251,#3252,#3253,#3254,#3255,
#3256,#3257,#3258,#3259,#3260,#3261,#3262,#3263,#3264,#3265,#3266,#3267,
#3268,#3269,#3270,#3271,#3272,#3273));
#752=EDGE_LOOP('',(#3274,#3275,#3276,#3277,#3278,#3279,#3280,#3281,#3282,
#3283,#3284,#3285,#3286,#3287,#3288,#3289,#3290,#3291,#3292,#3293,#3294,
#3295,#3296,#3297,#3298,#3299,#3300,#3301,#3302,#3303,#3304,#3305,#3306,
#3307,#3308,#3309,#3310,#3311,#3312,#3313,#3314,#3315,#3316,#3317,#3318,
#3319,#3320,#3321,#3322,#3323,#3324));
#753=EDGE_LOOP('',(#3325,#3326,#3327,#3328,#3329));
#754=EDGE_LOOP('',(#3330));
#755=EDGE_LOOP('',(#3331,#3332,#3333,#3334,#3335));
#756=EDGE_LOOP('',(#3336,#3337,#3338,#3339));
#757=EDGE_LOOP('',(#3340,#3341,#3342,#3343));
#758=EDGE_LOOP('',(#3344));
#759=EDGE_LOOP('',(#3345,#3346,#3347,#3348));
#760=EDGE_LOOP('',(#3349,#3350,#3351,#3352));
#761=EDGE_LOOP('',(#3353,#3354,#3355,#3356));
#762=EDGE_LOOP('',(#3357,#3358,#3359,#3360));
#763=EDGE_LOOP('',(#3361,#3362,#3363,#3364));
#764=EDGE_LOOP('',(#3365,#3366,#3367,#3368));
#765=EDGE_LOOP('',(#3369,#3370,#3371,#3372));
#766=EDGE_LOOP('',(#3373,#3374,#3375,#3376,#3377,#3378));
#767=EDGE_LOOP('',(#3379));
#768=EDGE_LOOP('',(#3380,#3381,#3382,#3383,#3384,#3385));
#769=EDGE_LOOP('',(#3386));
#770=EDGE_LOOP('',(#3387,#3388,#3389,#3390));
#771=EDGE_LOOP('',(#3391,#3392,#3393,#3394));
#772=EDGE_LOOP('',(#3395,#3396,#3397,#3398));
#773=EDGE_LOOP('',(#3399,#3400,#3401,#3402));
#774=EDGE_LOOP('',(#3403,#3404,#3405,#3406,#3407,#3408,#3409,#3410));
#775=EDGE_LOOP('',(#3411,#3412,#3413,#3414));
#776=EDGE_LOOP('',(#3415,#3416,#3417,#3418));
#777=EDGE_LOOP('',(#3419,#3420,#3421,#3422,#3423,#3424,#3425,#3426,#3427));
#778=EDGE_LOOP('',(#3428));
#779=EDGE_LOOP('',(#3429));
#780=EDGE_LOOP('',(#3430));
#781=EDGE_LOOP('',(#3431,#3432,#3433,#3434));
#782=EDGE_LOOP('',(#3435));
#783=EDGE_LOOP('',(#3436));
#784=EDGE_LOOP('',(#3437,#3438,#3439,#3440));
#785=EDGE_LOOP('',(#3441));
#786=EDGE_LOOP('',(#3442));
#787=EDGE_LOOP('',(#3443,#3444,#3445,#3446));
#788=EDGE_LOOP('',(#3447));
#789=EDGE_LOOP('',(#3448));
#790=EDGE_LOOP('',(#3449,#3450,#3451,#3452));
#791=EDGE_LOOP('',(#3453));
#792=EDGE_LOOP('',(#3454,#3455,#3456,#3457));
#793=EDGE_LOOP('',(#3458,#3459,#3460,#3461));
#794=EDGE_LOOP('',(#3462,#3463,#3464,#3465));
#795=EDGE_LOOP('',(#3466,#3467,#3468,#3469));
#796=EDGE_LOOP('',(#3470,#3471,#3472,#3473));
#797=EDGE_LOOP('',(#3474,#3475,#3476,#3477));
#798=EDGE_LOOP('',(#3478,#3479,#3480,#3481));
#799=EDGE_LOOP('',(#3482,#3483,#3484,#3485,#3486,#3487,#3488,#3489,#3490));
#800=EDGE_LOOP('',(#3491));
#801=EDGE_LOOP('',(#3492));
#802=EDGE_LOOP('',(#3493,#3494,#3495,#3496,#3497,#3498,#3499,#3500,#3501));
#803=EDGE_LOOP('',(#3502));
#804=EDGE_LOOP('',(#3503));
#805=EDGE_LOOP('',(#3504,#3505,#3506,#3507));
#806=EDGE_LOOP('',(#3508,#3509,#3510,#3511));
#807=EDGE_LOOP('',(#3512,#3513,#3514,#3515));
#808=EDGE_LOOP('',(#3516,#3517,#3518,#3519,#3520,#3521,#3522,#3523,#3524));
#809=EDGE_LOOP('',(#3525));
#810=EDGE_LOOP('',(#3526));
#811=EDGE_LOOP('',(#3527,#3528,#3529,#3530));
#812=EDGE_LOOP('',(#3531,#3532,#3533,#3534));
#813=EDGE_LOOP('',(#3535,#3536,#3537,#3538));
#814=EDGE_LOOP('',(#3539,#3540,#3541,#3542,#3543,#3544,#3545,#3546,#3547,
#3548));
#815=EDGE_LOOP('',(#3549,#3550,#3551,#3552));
#816=EDGE_LOOP('',(#3553,#3554,#3555,#3556));
#817=EDGE_LOOP('',(#3557,#3558,#3559,#3560));
#818=EDGE_LOOP('',(#3561,#3562,#3563,#3564));
#819=EDGE_LOOP('',(#3565,#3566,#3567,#3568));
#820=EDGE_LOOP('',(#3569,#3570,#3571,#3572));
#821=EDGE_LOOP('',(#3573,#3574,#3575,#3576,#3577,#3578,#3579,#3580,#3581));
#822=EDGE_LOOP('',(#3582));
#823=EDGE_LOOP('',(#3583));
#824=EDGE_LOOP('',(#3584,#3585,#3586,#3587));
#825=EDGE_LOOP('',(#3588,#3589,#3590,#3591));
#826=EDGE_LOOP('',(#3592,#3593,#3594,#3595));
#827=EDGE_LOOP('',(#3596,#3597,#3598,#3599));
#828=EDGE_LOOP('',(#3600,#3601,#3602,#3603,#3604,#3605,#3606,#3607));
#829=EDGE_LOOP('',(#3608,#3609,#3610,#3611,#3612,#3613,#3614));
#830=EDGE_LOOP('',(#3615,#3616,#3617,#3618));
#831=EDGE_LOOP('',(#3619,#3620,#3621,#3622));
#832=EDGE_LOOP('',(#3623,#3624,#3625,#3626));
#833=EDGE_LOOP('',(#3627,#3628,#3629,#3630));
#834=EDGE_LOOP('',(#3631,#3632,#3633,#3634));
#835=EDGE_LOOP('',(#3635,#3636,#3637,#3638,#3639,#3640,#3641,#3642));
#836=EDGE_LOOP('',(#3643,#3644,#3645,#3646,#3647,#3648,#3649));
#837=EDGE_LOOP('',(#3650,#3651,#3652,#3653));
#838=EDGE_LOOP('',(#3654,#3655,#3656,#3657));
#839=EDGE_LOOP('',(#3658,#3659,#3660,#3661));
#840=EDGE_LOOP('',(#3662,#3663,#3664,#3665));
#841=EDGE_LOOP('',(#3666,#3667,#3668,#3669,#3670,#3671,#3672,#3673,#3674));
#842=EDGE_LOOP('',(#3675));
#843=EDGE_LOOP('',(#3676));
#844=EDGE_LOOP('',(#3677,#3678,#3679,#3680));
#845=EDGE_LOOP('',(#3681,#3682,#3683,#3684));
#846=EDGE_LOOP('',(#3685,#3686,#3687,#3688));
#847=EDGE_LOOP('',(#3689,#3690,#3691,#3692));
#848=EDGE_LOOP('',(#3693,#3694,#3695,#3696));
#849=EDGE_LOOP('',(#3697,#3698,#3699,#3700,#3701));
#850=EDGE_LOOP('',(#3702,#3703,#3704,#3705,#3706));
#851=EDGE_LOOP('',(#3707,#3708,#3709,#3710));
#852=EDGE_LOOP('',(#3711,#3712,#3713,#3714));
#853=EDGE_LOOP('',(#3715,#3716,#3717,#3718));
#854=EDGE_LOOP('',(#3719,#3720,#3721,#3722));
#855=EDGE_LOOP('',(#3723,#3724,#3725,#3726));
#856=EDGE_LOOP('',(#3727,#3728,#3729,#3730));
#857=EDGE_LOOP('',(#3731,#3732,#3733,#3734,#3735));
#858=EDGE_LOOP('',(#3736,#3737,#3738,#3739));
#859=EDGE_LOOP('',(#3740,#3741,#3742,#3743));
#860=EDGE_LOOP('',(#3744,#3745,#3746,#3747));
#861=EDGE_LOOP('',(#3748,#3749,#3750,#3751,#3752,#3753,#3754,#3755,#3756,
#3757));
#862=EDGE_LOOP('',(#3758,#3759,#3760,#3761));
#863=EDGE_LOOP('',(#3762,#3763,#3764));
#864=EDGE_LOOP('',(#3765,#3766,#3767,#3768));
#865=EDGE_LOOP('',(#3769,#3770,#3771,#3772));
#866=EDGE_LOOP('',(#3773,#3774,#3775,#3776));
#867=EDGE_LOOP('',(#3777,#3778,#3779,#3780));
#868=EDGE_LOOP('',(#3781,#3782,#3783));
#869=EDGE_LOOP('',(#3784,#3785,#3786,#3787,#3788));
#870=EDGE_LOOP('',(#3789,#3790,#3791,#3792));
#871=EDGE_LOOP('',(#3793,#3794,#3795,#3796));
#872=EDGE_LOOP('',(#3797,#3798,#3799));
#873=EDGE_LOOP('',(#3800,#3801,#3802,#3803));
#874=EDGE_LOOP('',(#3804,#3805,#3806));
#875=EDGE_LOOP('',(#3807,#3808,#3809,#3810));
#876=EDGE_LOOP('',(#3811,#3812,#3813,#3814));
#877=EDGE_LOOP('',(#3815,#3816,#3817,#3818,#3819));
#878=EDGE_LOOP('',(#3820,#3821,#3822,#3823));
#879=EDGE_LOOP('',(#3824,#3825,#3826,#3827));
#880=EDGE_LOOP('',(#3828,#3829,#3830,#3831));
#881=EDGE_LOOP('',(#3832,#3833,#3834,#3835,#3836));
#882=EDGE_LOOP('',(#3837,#3838,#3839,#3840));
#883=LINE('',#5781,#1168);
#884=LINE('',#5787,#1169);
#885=LINE('',#5794,#1170);
#886=LINE('',#5797,#1171);
#887=LINE('',#5800,#1172);
#888=LINE('',#5802,#1173);
#889=LINE('',#5803,#1174);
#890=LINE('',#5809,#1175);
#891=LINE('',#5811,#1176);
#892=LINE('',#5812,#1177);
#893=LINE('',#5835,#1178);
#894=LINE('',#5838,#1179);
#895=LINE('',#5841,#1180);
#896=LINE('',#5845,#1181);
#897=LINE('',#5849,#1182);
#898=LINE('',#5857,#1183);
#899=LINE('',#5861,#1184);
#900=LINE('',#5864,#1185);
#901=LINE('',#5867,#1186);
#902=LINE('',#5870,#1187);
#903=LINE('',#5873,#1188);
#904=LINE('',#5874,#1189);
#905=LINE('',#5879,#1190);
#906=LINE('',#5880,#1191);
#907=LINE('',#5883,#1192);
#908=LINE('',#5884,#1193);
#909=LINE('',#5888,#1194);
#910=LINE('',#5891,#1195);
#911=LINE('',#5892,#1196);
#912=LINE('',#5895,#1197);
#913=LINE('',#5898,#1198);
#914=LINE('',#5901,#1199);
#915=LINE('',#5902,#1200);
#916=LINE('',#5907,#1201);
#917=LINE('',#5908,#1202);
#918=LINE('',#5910,#1203);
#919=LINE('',#5914,#1204);
#920=LINE('',#5919,#1205);
#921=LINE('',#5921,#1206);
#922=LINE('',#5923,#1207);
#923=LINE('',#5924,#1208);
#924=LINE('',#5927,#1209);
#925=LINE('',#5928,#1210);
#926=LINE('',#5929,#1211);
#927=LINE('',#5934,#1212);
#928=LINE('',#5936,#1213);
#929=LINE('',#5938,#1214);
#930=LINE('',#5939,#1215);
#931=LINE('',#5945,#1216);
#932=LINE('',#5948,#1217);
#933=LINE('',#5950,#1218);
#934=LINE('',#5951,#1219);
#935=LINE('',#5958,#1220);
#936=LINE('',#5960,#1221);
#937=LINE('',#5962,#1222);
#938=LINE('',#5963,#1223);
#939=LINE('',#5969,#1224);
#940=LINE('',#5972,#1225);
#941=LINE('',#5974,#1226);
#942=LINE('',#5975,#1227);
#943=LINE('',#5981,#1228);
#944=LINE('',#5983,#1229);
#945=LINE('',#5984,#1230);
#946=LINE('',#5990,#1231);
#947=LINE('',#5993,#1232);
#948=LINE('',#5995,#1233);
#949=LINE('',#5996,#1234);
#950=LINE('',#6022,#1235);
#951=LINE('',#6025,#1236);
#952=LINE('',#6028,#1237);
#953=LINE('',#6032,#1238);
#954=LINE('',#6035,#1239);
#955=LINE('',#6040,#1240);
#956=LINE('',#6043,#1241);
#957=LINE('',#6048,#1242);
#958=LINE('',#6051,#1243);
#959=LINE('',#6057,#1244);
#960=LINE('',#6060,#1245);
#961=LINE('',#6063,#1246);
#962=LINE('',#6065,#1247);
#963=LINE('',#6066,#1248);
#964=LINE('',#6069,#1249);
#965=LINE('',#6073,#1250);
#966=LINE('',#6077,#1251);
#967=LINE('',#6084,#1252);
#968=LINE('',#6087,#1253);
#969=LINE('',#6092,#1254);
#970=LINE('',#6093,#1255);
#971=LINE('',#6096,#1256);
#972=LINE('',#6097,#1257);
#973=LINE('',#6101,#1258);
#974=LINE('',#6104,#1259);
#975=LINE('',#6105,#1260);
#976=LINE('',#6108,#1261);
#977=LINE('',#6111,#1262);
#978=LINE('',#6114,#1263);
#979=LINE('',#6115,#1264);
#980=LINE('',#6120,#1265);
#981=LINE('',#6121,#1266);
#982=LINE('',#6123,#1267);
#983=LINE('',#6127,#1268);
#984=LINE('',#6132,#1269);
#985=LINE('',#6134,#1270);
#986=LINE('',#6135,#1271);
#987=LINE('',#6137,#1272);
#988=LINE('',#6139,#1273);
#989=LINE('',#6140,#1274);
#990=LINE('',#6145,#1275);
#991=LINE('',#6146,#1276);
#992=LINE('',#6147,#1277);
#993=LINE('',#6151,#1278);
#994=LINE('',#6154,#1279);
#995=LINE('',#6155,#1280);
#996=LINE('',#6161,#1281);
#997=LINE('',#6162,#1282);
#998=LINE('',#6163,#1283);
#999=LINE('',#6167,#1284);
#1000=LINE('',#6170,#1285);
#1001=LINE('',#6171,#1286);
#1002=LINE('',#6176,#1287);
#1003=LINE('',#6177,#1288);
#1004=LINE('',#6181,#1289);
#1005=LINE('',#6184,#1290);
#1006=LINE('',#6185,#1291);
#1007=LINE('',#6194,#1292);
#1008=LINE('',#6199,#1293);
#1009=LINE('',#6201,#1294);
#1010=LINE('',#6203,#1295);
#1011=LINE('',#6204,#1296);
#1012=LINE('',#6207,#1297);
#1013=LINE('',#6209,#1298);
#1014=LINE('',#6210,#1299);
#1015=LINE('',#6213,#1300);
#1016=LINE('',#6215,#1301);
#1017=LINE('',#6216,#1302);
#1018=LINE('',#6219,#1303);
#1019=LINE('',#6221,#1304);
#1020=LINE('',#6222,#1305);
#1021=LINE('',#6225,#1306);
#1022=LINE('',#6227,#1307);
#1023=LINE('',#6228,#1308);
#1024=LINE('',#6230,#1309);
#1025=LINE('',#6231,#1310);
#1026=LINE('',#6238,#1311);
#1027=LINE('',#6569,#1312);
#1028=LINE('',#6799,#1313);
#1029=LINE('',#7028,#1314);
#1030=LINE('',#7441,#1315);
#1031=LINE('',#7911,#1316);
#1032=LINE('',#8401,#1317);
#1033=LINE('',#8808,#1318);
#1034=LINE('',#9043,#1319);
#1035=LINE('',#9283,#1320);
#1036=LINE('',#9769,#1321);
#1037=LINE('',#10260,#1322);
#1038=LINE('',#10686,#1323);
#1039=LINE('',#11195,#1324);
#1040=LINE('',#11679,#1325);
#1041=LINE('',#11919,#1326);
#1042=LINE('',#12152,#1327);
#1043=LINE('',#12563,#1328);
#1044=LINE('',#13025,#1329);
#1045=LINE('',#13525,#1330);
#1046=LINE('',#13938,#1331);
#1047=LINE('',#14169,#1332);
#1048=LINE('',#21498,#1333);
#1049=LINE('',#21501,#1334);
#1050=LINE('',#21509,#1335);
#1051=LINE('',#21514,#1336);
#1052=LINE('',#21516,#1337);
#1053=LINE('',#21518,#1338);
#1054=LINE('',#21519,#1339);
#1055=LINE('',#21522,#1340);
#1056=LINE('',#21524,#1341);
#1057=LINE('',#21525,#1342);
#1058=LINE('',#21528,#1343);
#1059=LINE('',#21530,#1344);
#1060=LINE('',#21531,#1345);
#1061=LINE('',#21534,#1346);
#1062=LINE('',#21536,#1347);
#1063=LINE('',#21537,#1348);
#1064=LINE('',#21540,#1349);
#1065=LINE('',#21542,#1350);
#1066=LINE('',#21543,#1351);
#1067=LINE('',#21545,#1352);
#1068=LINE('',#21546,#1353);
#1069=LINE('',#21587,#1354);
#1070=LINE('',#21590,#1355);
#1071=LINE('',#21593,#1356);
#1072=LINE('',#21599,#1357);
#1073=LINE('',#21601,#1358);
#1074=LINE('',#21603,#1359);
#1075=LINE('',#21637,#1360);
#1076=LINE('',#21700,#1361);
#1077=LINE('',#21743,#1362);
#1078=LINE('',#21747,#1363);
#1079=LINE('',#21751,#1364);
#1080=LINE('',#21753,#1365);
#1081=LINE('',#21754,#1366);
#1082=LINE('',#21923,#1367);
#1083=LINE('',#21980,#1368);
#1084=LINE('',#21985,#1369);
#1085=LINE('',#21991,#1370);
#1086=LINE('',#21997,#1371);
#1087=LINE('',#22000,#1372);
#1088=LINE('',#22002,#1373);
#1089=LINE('',#22008,#1374);
#1090=LINE('',#22009,#1375);
#1091=LINE('',#22012,#1376);
#1092=LINE('',#22016,#1377);
#1093=LINE('',#22020,#1378);
#1094=LINE('',#22083,#1379);
#1095=LINE('',#22089,#1380);
#1096=LINE('',#22091,#1381);
#1097=LINE('',#22093,#1382);
#1098=LINE('',#22095,#1383);
#1099=LINE('',#22206,#1384);
#1100=LINE('',#22208,#1385);
#1101=LINE('',#22210,#1386);
#1102=LINE('',#22276,#1387);
#1103=LINE('',#22298,#1388);
#1104=LINE('',#22333,#1389);
#1105=LINE('',#22352,#1390);
#1106=LINE('',#22370,#1391);
#1107=LINE('',#22392,#1392);
#1108=LINE('',#22394,#1393);
#1109=LINE('',#22399,#1394);
#1110=LINE('',#22406,#1395);
#1111=LINE('',#22408,#1396);
#1112=LINE('',#22409,#1397);
#1113=LINE('',#22413,#1398);
#1114=LINE('',#22415,#1399);
#1115=LINE('',#22417,#1400);
#1116=LINE('',#22418,#1401);
#1117=LINE('',#22420,#1402);
#1118=LINE('',#22421,#1403);
#1119=LINE('',#22468,#1404);
#1120=LINE('',#22487,#1405);
#1121=LINE('',#22489,#1406);
#1122=LINE('',#22512,#1407);
#1123=LINE('',#22517,#1408);
#1124=LINE('',#22518,#1409);
#1125=LINE('',#22560,#1410);
#1126=LINE('',#22583,#1411);
#1127=LINE('',#22584,#1412);
#1128=LINE('',#22587,#1413);
#1129=LINE('',#22591,#1414);
#1130=LINE('',#22594,#1415);
#1131=LINE('',#22597,#1416);
#1132=LINE('',#22603,#1417);
#1133=LINE('',#22625,#1418);
#1134=LINE('',#22627,#1419);
#1135=LINE('',#22629,#1420);
#1136=LINE('',#22634,#1421);
#1137=LINE('',#22638,#1422);
#1138=LINE('',#22640,#1423);
#1139=LINE('',#22681,#1424);
#1140=LINE('',#22682,#1425);
#1141=LINE('',#22685,#1426);
#1142=LINE('',#22688,#1427);
#1143=LINE('',#22690,#1428);
#1144=LINE('',#22877,#1429);
#1145=LINE('',#22878,#1430);
#1146=LINE('',#22928,#1431);
#1147=LINE('',#22929,#1432);
#1148=LINE('',#22969,#1433);
#1149=LINE('',#22970,#1434);
#1150=LINE('',#22972,#1435);
#1151=LINE('',#22973,#1436);
#1152=LINE('',#22978,#1437);
#1153=LINE('',#22998,#1438);
#1154=LINE('',#23005,#1439);
#1155=LINE('',#23007,#1440);
#1156=LINE('',#23008,#1441);
#1157=LINE('',#23114,#1442);
#1158=LINE('',#23116,#1443);
#1159=LINE('',#23128,#1444);
#1160=LINE('',#23131,#1445);
#1161=LINE('',#23173,#1446);
#1162=LINE('',#23270,#1447);
#1163=LINE('',#23274,#1448);
#1164=LINE('',#23436,#1449);
#1165=LINE('',#23440,#1450);
#1166=LINE('',#23444,#1451);
#1167=LINE('',#23445,#1452);
#1168=VECTOR('',#4682,1.75974879114541);
#1169=VECTOR('',#4689,1.69478250292167);
#1170=VECTOR('',#4696,10.);
#1171=VECTOR('',#4699,10.);
#1172=VECTOR('',#4702,10.);
#1173=VECTOR('',#4703,10.);
#1174=VECTOR('',#4704,10.);
#1175=VECTOR('',#4711,10.);
#1176=VECTOR('',#4714,10.);
#1177=VECTOR('',#4715,10.);
#1178=VECTOR('',#4746,10.);
#1179=VECTOR('',#4749,10.);
#1180=VECTOR('',#4752,9.99999999999999);
#1181=VECTOR('',#4755,10.);
#1182=VECTOR('',#4758,10.);
#1183=VECTOR('',#4765,10.);
#1184=VECTOR('',#4768,10.);
#1185=VECTOR('',#4771,9.99999999999999);
#1186=VECTOR('',#4774,10.);
#1187=VECTOR('',#4777,10.);
#1188=VECTOR('',#4780,10.);
#1189=VECTOR('',#4781,10.);
#1190=VECTOR('',#4786,10.);
#1191=VECTOR('',#4787,10.);
#1192=VECTOR('',#4790,10.);
#1193=VECTOR('',#4791,10.);
#1194=VECTOR('',#4796,10.);
#1195=VECTOR('',#4799,10.);
#1196=VECTOR('',#4800,9.99999999999999);
#1197=VECTOR('',#4803,10.);
#1198=VECTOR('',#4806,10.);
#1199=VECTOR('',#4809,9.99999999999999);
#1200=VECTOR('',#4810,10.);
#1201=VECTOR('',#4815,10.);
#1202=VECTOR('',#4816,10.);
#1203=VECTOR('',#4819,10.);
#1204=VECTOR('',#4824,10.);
#1205=VECTOR('',#4831,10.);
#1206=VECTOR('',#4832,10.);
#1207=VECTOR('',#4833,10.);
#1208=VECTOR('',#4834,10.);
#1209=VECTOR('',#4837,10.);
#1210=VECTOR('',#4838,10.);
#1211=VECTOR('',#4839,10.);
#1212=VECTOR('',#4844,10.);
#1213=VECTOR('',#4845,10.);
#1214=VECTOR('',#4846,10.);
#1215=VECTOR('',#4847,10.);
#1216=VECTOR('',#4854,10.);
#1217=VECTOR('',#4857,10.);
#1218=VECTOR('',#4858,10.);
#1219=VECTOR('',#4859,10.);
#1220=VECTOR('',#4868,10.);
#1221=VECTOR('',#4869,10.);
#1222=VECTOR('',#4870,10.);
#1223=VECTOR('',#4871,10.);
#1224=VECTOR('',#4878,10.);
#1225=VECTOR('',#4881,10.);
#1226=VECTOR('',#4882,10.);
#1227=VECTOR('',#4883,10.);
#1228=VECTOR('',#4892,10.);
#1229=VECTOR('',#4893,10.);
#1230=VECTOR('',#4894,10.);
#1231=VECTOR('',#4901,10.);
#1232=VECTOR('',#4904,10.);
#1233=VECTOR('',#4905,10.);
#1234=VECTOR('',#4906,10.);
#1235=VECTOR('',#4943,10.);
#1236=VECTOR('',#4946,10.);
#1237=VECTOR('',#4949,10.);
#1238=VECTOR('',#4952,10.);
#1239=VECTOR('',#4955,10.);
#1240=VECTOR('',#4958,10.);
#1241=VECTOR('',#4961,10.);
#1242=VECTOR('',#4964,10.);
#1243=VECTOR('',#4967,10.);
#1244=VECTOR('',#4972,10.);
#1245=VECTOR('',#4975,10.);
#1246=VECTOR('',#4978,10.);
#1247=VECTOR('',#4979,10.);
#1248=VECTOR('',#4980,10.);
#1249=VECTOR('',#4983,9.99999999999999);
#1250=VECTOR('',#4986,10.);
#1251=VECTOR('',#4989,10.);
#1252=VECTOR('',#4996,10.);
#1253=VECTOR('',#4999,9.99999999999999);
#1254=VECTOR('',#5004,10.);
#1255=VECTOR('',#5005,10.);
#1256=VECTOR('',#5008,10.);
#1257=VECTOR('',#5009,10.);
#1258=VECTOR('',#5014,10.);
#1259=VECTOR('',#5017,9.99999999999999);
#1260=VECTOR('',#5018,10.);
#1261=VECTOR('',#5021,10.);
#1262=VECTOR('',#5024,10.);
#1263=VECTOR('',#5027,10.);
#1264=VECTOR('',#5028,9.99999999999999);
#1265=VECTOR('',#5033,10.);
#1266=VECTOR('',#5034,10.);
#1267=VECTOR('',#5037,10.);
#1268=VECTOR('',#5042,10.);
#1269=VECTOR('',#5049,10.);
#1270=VECTOR('',#5050,10.);
#1271=VECTOR('',#5051,10.);
#1272=VECTOR('',#5054,10.);
#1273=VECTOR('',#5055,10.);
#1274=VECTOR('',#5056,10.);
#1275=VECTOR('',#5061,10.);
#1276=VECTOR('',#5062,10.);
#1277=VECTOR('',#5063,10.);
#1278=VECTOR('',#5068,10.);
#1279=VECTOR('',#5071,10.);
#1280=VECTOR('',#5072,10.);
#1281=VECTOR('',#5079,10.);
#1282=VECTOR('',#5080,10.);
#1283=VECTOR('',#5081,10.);
#1284=VECTOR('',#5086,10.);
#1285=VECTOR('',#5089,10.);
#1286=VECTOR('',#5090,10.);
#1287=VECTOR('',#5097,10.);
#1288=VECTOR('',#5098,10.);
#1289=VECTOR('',#5103,10.);
#1290=VECTOR('',#5106,10.);
#1291=VECTOR('',#5107,10.);
#1292=VECTOR('',#5120,2.5);
#1293=VECTOR('',#5125,9.99999999999999);
#1294=VECTOR('',#5126,10.);
#1295=VECTOR('',#5127,9.99999999999999);
#1296=VECTOR('',#5128,10.);
#1297=VECTOR('',#5131,10.);
#1298=VECTOR('',#5132,10.);
#1299=VECTOR('',#5133,10.);
#1300=VECTOR('',#5136,10.);
#1301=VECTOR('',#5137,10.);
#1302=VECTOR('',#5138,10.);
#1303=VECTOR('',#5141,10.);
#1304=VECTOR('',#5142,10.);
#1305=VECTOR('',#5143,10.);
#1306=VECTOR('',#5146,10.);
#1307=VECTOR('',#5147,10.);
#1308=VECTOR('',#5148,10.);
#1309=VECTOR('',#5151,10.);
#1310=VECTOR('',#5152,10.);
#1311=VECTOR('',#5161,1.99475);
#1312=VECTOR('',#5166,1.99475);
#1313=VECTOR('',#5169,1.99475);
#1314=VECTOR('',#5172,1.99475);
#1315=VECTOR('',#5175,1.99475);
#1316=VECTOR('',#5178,1.99475);
#1317=VECTOR('',#5181,1.99475);
#1318=VECTOR('',#5184,1.99475);
#1319=VECTOR('',#5187,1.99475);
#1320=VECTOR('',#5190,1.99475);
#1321=VECTOR('',#5193,1.99475);
#1322=VECTOR('',#5196,1.99475);
#1323=VECTOR('',#5199,1.99475);
#1324=VECTOR('',#5202,1.99475);
#1325=VECTOR('',#5205,1.99475);
#1326=VECTOR('',#5208,1.99475);
#1327=VECTOR('',#5211,1.99475);
#1328=VECTOR('',#5214,1.99475);
#1329=VECTOR('',#5217,1.99475);
#1330=VECTOR('',#5220,1.99475);
#1331=VECTOR('',#5223,1.99475);
#1332=VECTOR('',#5226,1.99475);
#1333=VECTOR('',#5247,5.14028464662889);
#1334=VECTOR('',#5250,6.05319927020769);
#1335=VECTOR('',#5261,2.5);
#1336=VECTOR('',#5266,9.99999999999999);
#1337=VECTOR('',#5267,10.);
#1338=VECTOR('',#5268,9.99999999999999);
#1339=VECTOR('',#5269,10.);
#1340=VECTOR('',#5272,10.);
#1341=VECTOR('',#5273,10.);
#1342=VECTOR('',#5274,10.);
#1343=VECTOR('',#5277,10.);
#1344=VECTOR('',#5278,10.);
#1345=VECTOR('',#5279,10.);
#1346=VECTOR('',#5282,10.);
#1347=VECTOR('',#5283,10.);
#1348=VECTOR('',#5284,10.);
#1349=VECTOR('',#5287,10.);
#1350=VECTOR('',#5288,10.);
#1351=VECTOR('',#5289,10.);
#1352=VECTOR('',#5292,10.);
#1353=VECTOR('',#5293,10.);
#1354=VECTOR('',#5316,10.);
#1355=VECTOR('',#5319,10.);
#1356=VECTOR('',#5322,10.);
#1357=VECTOR('',#5329,10.);
#1358=VECTOR('',#5330,10.);
#1359=VECTOR('',#5331,10.);
#1360=VECTOR('',#5346,10.);
#1361=VECTOR('',#5353,10.);
#1362=VECTOR('',#5412,1.69478250292167);
#1363=VECTOR('',#5417,1.70133516896762);
#1364=VECTOR('',#5422,10.);
#1365=VECTOR('',#5423,10.);
#1366=VECTOR('',#5424,10.);
#1367=VECTOR('',#5425,10.);
#1368=VECTOR('',#5426,10.);
#1369=VECTOR('',#5431,10.);
#1370=VECTOR('',#5438,10.);
#1371=VECTOR('',#5449,10.);
#1372=VECTOR('',#5452,10.);
#1373=VECTOR('',#5453,10.);
#1374=VECTOR('',#5460,10.);
#1375=VECTOR('',#5461,10.);
#1376=VECTOR('',#5464,10.);
#1377=VECTOR('',#5469,10.);
#1378=VECTOR('',#5474,10.);
#1379=VECTOR('',#5481,10.);
#1380=VECTOR('',#5488,1.69478250292167);
#1381=VECTOR('',#5491,1.70133516896762);
#1382=VECTOR('',#5494,10.);
#1383=VECTOR('',#5497,10.);
#1384=VECTOR('',#5498,10.);
#1385=VECTOR('',#5501,10.);
#1386=VECTOR('',#5504,10.);
#1387=VECTOR('',#5509,10.);
#1388=VECTOR('',#5510,10.);
#1389=VECTOR('',#5511,10.);
#1390=VECTOR('',#5512,10.);
#1391=VECTOR('',#5517,10.);
#1392=VECTOR('',#5518,10.);
#1393=VECTOR('',#5519,10.);
#1394=VECTOR('',#5524,10.);
#1395=VECTOR('',#5531,10.);
#1396=VECTOR('',#5532,10.);
#1397=VECTOR('',#5533,10.);
#1398=VECTOR('',#5536,10.);
#1399=VECTOR('',#5537,10.);
#1400=VECTOR('',#5538,10.);
#1401=VECTOR('',#5539,10.);
#1402=VECTOR('',#5542,10.);
#1403=VECTOR('',#5543,10.);
#1404=VECTOR('',#5544,10.);
#1405=VECTOR('',#5547,10.);
#1406=VECTOR('',#5548,10.);
#1407=VECTOR('',#5549,10.);
#1408=VECTOR('',#5554,10.);
#1409=VECTOR('',#5555,10.);
#1410=VECTOR('',#5556,10.);
#1411=VECTOR('',#5559,10.);
#1412=VECTOR('',#5560,10.);
#1413=VECTOR('',#5563,10.);
#1414=VECTOR('',#5568,10.);
#1415=VECTOR('',#5571,10.);
#1416=VECTOR('',#5574,10.);
#1417=VECTOR('',#5581,10.);
#1418=VECTOR('',#5582,10.);
#1419=VECTOR('',#5583,10.);
#1420=VECTOR('',#5584,10.);
#1421=VECTOR('',#5591,1.70133516896762);
#1422=VECTOR('',#5596,1.70133516896762);
#1423=VECTOR('',#5599,10.);
#1424=VECTOR('',#5600,10.);
#1425=VECTOR('',#5601,10.);
#1426=VECTOR('',#5606,10.);
#1427=VECTOR('',#5611,10.);
#1428=VECTOR('',#5614,10.);
#1429=VECTOR('',#5635,10.);
#1430=VECTOR('',#5636,10.);
#1431=VECTOR('',#5643,10.);
#1432=VECTOR('',#5644,10.);
#1433=VECTOR('',#5649,10.);
#1434=VECTOR('',#5650,10.);
#1435=VECTOR('',#5653,10.);
#1436=VECTOR('',#5654,10.);
#1437=VECTOR('',#5659,10.);
#1438=VECTOR('',#5672,10.);
#1439=VECTOR('',#5681,10.);
#1440=VECTOR('',#5682,10.);
#1441=VECTOR('',#5683,10.);
#1442=VECTOR('',#5700,10.);
#1443=VECTOR('',#5703,10.);
#1444=VECTOR('',#5704,10.);
#1445=VECTOR('',#5707,10.);
#1446=VECTOR('',#5708,10.);
#1447=VECTOR('',#5729,10.);
#1448=VECTOR('',#5736,10.);
#1449=VECTOR('',#5741,10.);
#1450=VECTOR('',#5746,10.);
#1451=VECTOR('',#5751,10.);
#1452=VECTOR('',#5752,10.);
#1453=CIRCLE('',#4269,1.75974879114541);
#1454=CIRCLE('',#4270,1.75974879114541);
#1455=CIRCLE('',#4272,1.69478250292167);
#1456=CIRCLE('',#4273,1.69478250292167);
#1457=CIRCLE('',#4275,2.25974879114541);
#1458=CIRCLE('',#4276,2.25974879114541);
#1459=CIRCLE('',#4279,2.69478250292167);
#1460=CIRCLE('',#4280,2.69478250292167);
#1461=CIRCLE('',#4286,1.70133516896762);
#1462=CIRCLE('',#4287,0.5);
#1463=CIRCLE('',#4288,2.20133516896762);
#1464=CIRCLE('',#4291,1.75974879114541);
#1465=CIRCLE('',#4292,0.5);
#1466=CIRCLE('',#4293,2.25974879114541);
#1467=CIRCLE('',#4299,2.75);
#1468=CIRCLE('',#4300,2.5);
#1469=CIRCLE('',#4301,2.00000000000029);
#1470=CIRCLE('',#4302,3.70283120062258);
#1471=CIRCLE('',#4303,2.00000000000029);
#1472=CIRCLE('',#4304,2.5);
#1473=CIRCLE('',#4305,2.75);
#1474=CIRCLE('',#4307,2.5);
#1475=CIRCLE('',#4310,2.5);
#1476=CIRCLE('',#4313,2.75);
#1477=CIRCLE('',#4316,2.75);
#1478=CIRCLE('',#4319,2.00000000000029);
#1479=CIRCLE('',#4322,2.00000000000029);
#1480=CIRCLE('',#4324,3.70283120062258);
#1481=CIRCLE('',#4330,2.29663666580012);
#1482=CIRCLE('',#4331,2.29663666580012);
#1483=CIRCLE('',#4334,2.29663666580012);
#1484=CIRCLE('',#4335,2.29663666580012);
#1485=CIRCLE('',#4338,2.29663666580012);
#1486=CIRCLE('',#4339,2.29663666580012);
#1487=CIRCLE('',#4342,2.29663666580012);
#1488=CIRCLE('',#4343,2.29663666580012);
#1489=CIRCLE('',#4346,2.50000000000001);
#1490=CIRCLE('',#4347,2.50000000000001);
#1491=CIRCLE('',#4350,2.5);
#1492=CIRCLE('',#4351,2.5);
#1493=CIRCLE('',#4356,1.70133516896762);
#1494=CIRCLE('',#4357,0.5);
#1495=CIRCLE('',#4358,2.20133516896762);
#1496=CIRCLE('',#4361,1.75974879114541);
#1497=CIRCLE('',#4362,0.5);
#1498=CIRCLE('',#4363,2.25974879114541);
#1499=CIRCLE('',#4369,2.50000000000001);
#1500=CIRCLE('',#4370,2.5);
#1501=CIRCLE('',#4371,2.29663666580012);
#1502=CIRCLE('',#4372,2.29663666580012);
#1503=CIRCLE('',#4373,2.29663666580012);
#1504=CIRCLE('',#4374,2.29663666580012);
#1505=CIRCLE('',#4376,2.5);
#1506=CIRCLE('',#4377,2.5);
#1507=CIRCLE('',#4380,2.75);
#1508=CIRCLE('',#4381,2.5);
#1509=CIRCLE('',#4382,2.00000000000029);
#1510=CIRCLE('',#4383,3.70283120062258);
#1511=CIRCLE('',#4384,2.00000000000029);
#1512=CIRCLE('',#4385,2.75);
#1513=CIRCLE('',#4387,2.5);
#1514=CIRCLE('',#4390,2.75);
#1515=CIRCLE('',#4393,2.75);
#1516=CIRCLE('',#4396,2.00000000000029);
#1517=CIRCLE('',#4399,2.00000000000029);
#1518=CIRCLE('',#4401,3.70283120062258);
#1519=CIRCLE('',#4407,2.29663666580012);
#1520=CIRCLE('',#4410,2.29663666580012);
#1521=CIRCLE('',#4413,2.29663666580012);
#1522=CIRCLE('',#4416,2.29663666580012);
#1523=CIRCLE('',#4419,2.50000000000001);
#1524=CIRCLE('',#4422,2.5);
#1525=CIRCLE('',#4426,2.5);
#1526=CIRCLE('',#4427,2.5);
#1527=CIRCLE('',#4438,1.99475);
#1528=CIRCLE('',#4461,2.4505);
#1529=CIRCLE('',#4462,2.4505);
#1530=CIRCLE('',#4464,1.99475);
#1531=CIRCLE('',#4467,3.24975268099691);
#1532=CIRCLE('',#4469,7.03081661226087);
#1533=CIRCLE('',#4471,5.0755819281545);
#1534=CIRCLE('',#4475,2.5);
#1535=CIRCLE('',#4476,2.5);
#1536=CIRCLE('',#4487,63.3332952479771);
#1537=CIRCLE('',#4488,1.);
#1538=CIRCLE('',#4489,62.3332952479771);
#1539=CIRCLE('',#4491,49.7730300598817);
#1540=CIRCLE('',#4492,50.7730300598817);
#1541=CIRCLE('',#4494,62.3332952479771);
#1542=CIRCLE('',#4496,49.7730300598817);
#1543=CIRCLE('',#4498,1.6332945980533);
#1544=CIRCLE('',#4499,1.6332945980533);
#1545=CIRCLE('',#4501,1.);
#1546=CIRCLE('',#4502,63.3332952479771);
#1547=CIRCLE('',#4504,50.7730300598817);
#1548=CIRCLE('',#4506,2.8615696413584);
#1549=CIRCLE('',#4507,6.2515148621032);
#1550=CIRCLE('',#4508,2.81236096609945);
#1551=CIRCLE('',#4509,2.19478250292167);
#1552=CIRCLE('',#4510,2.20133516896762);
#1553=CIRCLE('',#4512,1.70133516896762);
#1554=CIRCLE('',#4514,1.49422838778107);
#1555=CIRCLE('',#4515,0.75);
#1556=CIRCLE('',#4518,1.69478250292167);
#1557=CIRCLE('',#4520,1.48767572173512);
#1558=CIRCLE('',#4521,0.75);
#1559=CIRCLE('',#4524,1.70133516896762);
#1560=CIRCLE('',#4526,1.49422838778107);
#1561=CIRCLE('',#4527,0.75);
#1562=CIRCLE('',#4528,2.20133516896762);
#1563=CIRCLE('',#4531,1.69478250292167);
#1564=CIRCLE('',#4533,1.48767572173512);
#1565=CIRCLE('',#4534,0.75);
#1566=CIRCLE('',#4535,2.19478250292167);
#1567=CIRCLE('',#4538,1.69478250292167);
#1568=CIRCLE('',#4540,1.70133516896762);
#1569=CIRCLE('',#4543,2.81236096609945);
#1570=CIRCLE('',#4544,2.81236096609945);
#1571=CIRCLE('',#4546,6.2515148621032);
#1572=CIRCLE('',#4547,6.2515148621032);
#1573=CIRCLE('',#4549,2.8615696413584);
#1574=CIRCLE('',#4550,2.8615696413584);
#1575=CIRCLE('',#4553,64.0604216491307);
#1576=CIRCLE('',#4554,51.5001564610352);
#1577=CIRCLE('',#4557,51.5001564610352);
#1578=CIRCLE('',#4559,64.0604216491307);
#1579=CIRCLE('',#4561,2.81236096609945);
#1580=CIRCLE('',#4562,6.2515148621032);
#1581=CIRCLE('',#4563,2.8615696413584);
#1582=CIRCLE('',#4564,1.69478250292167);
#1583=CIRCLE('',#4565,1.70133516896762);
#1584=CIRCLE('',#4575,2.8615696413584);
#1585=CIRCLE('',#4576,1.99589528357813);
#1586=CIRCLE('',#4577,2.8615696413584);
#1587=CIRCLE('',#4578,1.70133516896762);
#1588=CIRCLE('',#4579,1.70133516896762);
#1589=CIRCLE('',#4584,4.33051922028271);
#1590=CIRCLE('',#4585,2.66551922028271);
#1591=CIRCLE('',#4588,2.8615696413584);
#1592=CIRCLE('',#4590,2.8615696413584);
#1593=CIRCLE('',#4592,1.99589528357813);
#1594=CIRCLE('',#4594,4.33051922028271);
#1595=CIRCLE('',#4595,2.66551922028271);
#1596=CIRCLE('',#4597,1.70133516896762);
#1597=CIRCLE('',#4599,1.70133516896762);
#1598=CIRCLE('',#4608,0.499999999999996);
#1599=CIRCLE('',#4609,0.5);
#1600=CIRCLE('',#4611,0.499999999999996);
#1601=CIRCLE('',#4612,0.499999999999992);
#1602=CIRCLE('',#4615,0.499999999999995);
#1603=CIRCLE('',#4616,0.499999999999996);
#1604=CIRCLE('',#4618,0.499999999999987);
#1605=CIRCLE('',#4619,0.499999999999996);
#1606=CIRCLE('',#4623,62.8868723549169);
#1607=CIRCLE('',#4624,18.7866355153418);
#1608=CIRCLE('',#4626,61.8868723549169);
#1609=CIRCLE('',#4627,0.999999999999999);
#1610=CIRCLE('',#4629,61.8868723549169);
#1611=CIRCLE('',#4631,62.8868723549169);
#1612=CIRCLE('',#4632,1.);
#1613=CIRCLE('',#4634,1.);
#1614=CIRCLE('',#4636,1.00000000000001);
#1615=CIRCLE('',#4637,1.);
#1616=CIRCLE('',#4639,19.7866355153418);
#1617=CIRCLE('',#4640,18.7866355153418);
#1618=CIRCLE('',#4642,1.);
#1619=CIRCLE('',#4643,1.00000000000001);
#1620=CIRCLE('',#4645,0.999999999999998);
#1621=CIRCLE('',#4648,19.7866355153418);
#1622=CIRCLE('',#4649,1.);
#1623=CIRCLE('',#4651,1.);
#1624=CIRCLE('',#4653,1.);
#1625=CIRCLE('',#4655,0.999999999999998);
#1626=CIRCLE('',#4659,62.3332952479768);
#1627=CIRCLE('',#4661,62.3332952479768);
#1628=VERTEX_POINT('',#5778);
#1629=VERTEX_POINT('',#5780);
#1630=VERTEX_POINT('',#5784);
#1631=VERTEX_POINT('',#5786);
#1632=VERTEX_POINT('',#5790);
#1633=VERTEX_POINT('',#5791);
#1634=VERTEX_POINT('',#5793);
#1635=VERTEX_POINT('',#5795);
#1636=VERTEX_POINT('',#5799);
#1637=VERTEX_POINT('',#5801);
#1638=VERTEX_POINT('',#5805);
#1639=VERTEX_POINT('',#5807);
#1640=VERTEX_POINT('',#5817);
#1641=VERTEX_POINT('',#5819);
#1642=VERTEX_POINT('',#5824);
#1643=VERTEX_POINT('',#5826);
#1644=VERTEX_POINT('',#5831);
#1645=VERTEX_POINT('',#5832);
#1646=VERTEX_POINT('',#5834);
#1647=VERTEX_POINT('',#5836);
#1648=VERTEX_POINT('',#5840);
#1649=VERTEX_POINT('',#5842);
#1650=VERTEX_POINT('',#5844);
#1651=VERTEX_POINT('',#5846);
#1652=VERTEX_POINT('',#5848);
#1653=VERTEX_POINT('',#5850);
#1654=VERTEX_POINT('',#5852);
#1655=VERTEX_POINT('',#5854);
#1656=VERTEX_POINT('',#5856);
#1657=VERTEX_POINT('',#5858);
#1658=VERTEX_POINT('',#5860);
#1659=VERTEX_POINT('',#5862);
#1660=VERTEX_POINT('',#5866);
#1661=VERTEX_POINT('',#5868);
#1662=VERTEX_POINT('',#5872);
#1663=VERTEX_POINT('',#5876);
#1664=VERTEX_POINT('',#5877);
#1665=VERTEX_POINT('',#5882);
#1666=VERTEX_POINT('',#5886);
#1667=VERTEX_POINT('',#5890);
#1668=VERTEX_POINT('',#5894);
#1669=VERTEX_POINT('',#5896);
#1670=VERTEX_POINT('',#5900);
#1671=VERTEX_POINT('',#5904);
#1672=VERTEX_POINT('',#5905);
#1673=VERTEX_POINT('',#5912);
#1674=VERTEX_POINT('',#5918);
#1675=VERTEX_POINT('',#5920);
#1676=VERTEX_POINT('',#5922);
#1677=VERTEX_POINT('',#5926);
#1678=VERTEX_POINT('',#5932);
#1679=VERTEX_POINT('',#5933);
#1680=VERTEX_POINT('',#5935);
#1681=VERTEX_POINT('',#5937);
#1682=VERTEX_POINT('',#5941);
#1683=VERTEX_POINT('',#5943);
#1684=VERTEX_POINT('',#5947);
#1685=VERTEX_POINT('',#5949);
#1686=VERTEX_POINT('',#5956);
#1687=VERTEX_POINT('',#5957);
#1688=VERTEX_POINT('',#5959);
#1689=VERTEX_POINT('',#5961);
#1690=VERTEX_POINT('',#5965);
#1691=VERTEX_POINT('',#5967);
#1692=VERTEX_POINT('',#5971);
#1693=VERTEX_POINT('',#5973);
#1694=VERTEX_POINT('',#5980);
#1695=VERTEX_POINT('',#5982);
#1696=VERTEX_POINT('',#5986);
#1697=VERTEX_POINT('',#5988);
#1698=VERTEX_POINT('',#5992);
#1699=VERTEX_POINT('',#5994);
#1700=VERTEX_POINT('',#6004);
#1701=VERTEX_POINT('',#6006);
#1702=VERTEX_POINT('',#6011);
#1703=VERTEX_POINT('',#6013);
#1704=VERTEX_POINT('',#6018);
#1705=VERTEX_POINT('',#6019);
#1706=VERTEX_POINT('',#6021);
#1707=VERTEX_POINT('',#6023);
#1708=VERTEX_POINT('',#6027);
#1709=VERTEX_POINT('',#6029);
#1710=VERTEX_POINT('',#6031);
#1711=VERTEX_POINT('',#6033);
#1712=VERTEX_POINT('',#6036);
#1713=VERTEX_POINT('',#6037);
#1714=VERTEX_POINT('',#6039);
#1715=VERTEX_POINT('',#6041);
#1716=VERTEX_POINT('',#6044);
#1717=VERTEX_POINT('',#6045);
#1718=VERTEX_POINT('',#6047);
#1719=VERTEX_POINT('',#6049);
#1720=VERTEX_POINT('',#6053);
#1721=VERTEX_POINT('',#6054);
#1722=VERTEX_POINT('',#6056);
#1723=VERTEX_POINT('',#6058);
#1724=VERTEX_POINT('',#6062);
#1725=VERTEX_POINT('',#6064);
#1726=VERTEX_POINT('',#6068);
#1727=VERTEX_POINT('',#6070);
#1728=VERTEX_POINT('',#6072);
#1729=VERTEX_POINT('',#6074);
#1730=VERTEX_POINT('',#6076);
#1731=VERTEX_POINT('',#6078);
#1732=VERTEX_POINT('',#6080);
#1733=VERTEX_POINT('',#6082);
#1734=VERTEX_POINT('',#6085);
#1735=VERTEX_POINT('',#6089);
#1736=VERTEX_POINT('',#6090);
#1737=VERTEX_POINT('',#6095);
#1738=VERTEX_POINT('',#6099);
#1739=VERTEX_POINT('',#6103);
#1740=VERTEX_POINT('',#6107);
#1741=VERTEX_POINT('',#6109);
#1742=VERTEX_POINT('',#6113);
#1743=VERTEX_POINT('',#6117);
#1744=VERTEX_POINT('',#6118);
#1745=VERTEX_POINT('',#6125);
#1746=VERTEX_POINT('',#6131);
#1747=VERTEX_POINT('',#6133);
#1748=VERTEX_POINT('',#6138);
#1749=VERTEX_POINT('',#6143);
#1750=VERTEX_POINT('',#6144);
#1751=VERTEX_POINT('',#6149);
#1752=VERTEX_POINT('',#6153);
#1753=VERTEX_POINT('',#6159);
#1754=VERTEX_POINT('',#6160);
#1755=VERTEX_POINT('',#6165);
#1756=VERTEX_POINT('',#6169);
#1757=VERTEX_POINT('',#6175);
#1758=VERTEX_POINT('',#6179);
#1759=VERTEX_POINT('',#6183);
#1760=VERTEX_POINT('',#6191);
#1761=VERTEX_POINT('',#6193);
#1762=VERTEX_POINT('',#6197);
#1763=VERTEX_POINT('',#6198);
#1764=VERTEX_POINT('',#6200);
#1765=VERTEX_POINT('',#6202);
#1766=VERTEX_POINT('',#6206);
#1767=VERTEX_POINT('',#6208);
#1768=VERTEX_POINT('',#6212);
#1769=VERTEX_POINT('',#6214);
#1770=VERTEX_POINT('',#6218);
#1771=VERTEX_POINT('',#6220);
#1772=VERTEX_POINT('',#6224);
#1773=VERTEX_POINT('',#6226);
#1774=VERTEX_POINT('',#6236);
#1775=VERTEX_POINT('',#6237);
#1776=VERTEX_POINT('',#6239);
#1777=VERTEX_POINT('',#6440);
#1778=VERTEX_POINT('',#6567);
#1779=VERTEX_POINT('',#6568);
#1780=VERTEX_POINT('',#6797);
#1781=VERTEX_POINT('',#6798);
#1782=VERTEX_POINT('',#7026);
#1783=VERTEX_POINT('',#7027);
#1784=VERTEX_POINT('',#7439);
#1785=VERTEX_POINT('',#7440);
#1786=VERTEX_POINT('',#7909);
#1787=VERTEX_POINT('',#7910);
#1788=VERTEX_POINT('',#8399);
#1789=VERTEX_POINT('',#8400);
#1790=VERTEX_POINT('',#8806);
#1791=VERTEX_POINT('',#8807);
#1792=VERTEX_POINT('',#9041);
#1793=VERTEX_POINT('',#9042);
#1794=VERTEX_POINT('',#9281);
#1795=VERTEX_POINT('',#9282);
#1796=VERTEX_POINT('',#9767);
#1797=VERTEX_POINT('',#9768);
#1798=VERTEX_POINT('',#9982);
#1799=VERTEX_POINT('',#10258);
#1800=VERTEX_POINT('',#10259);
#1801=VERTEX_POINT('',#10684);
#1802=VERTEX_POINT('',#10685);
#1803=VERTEX_POINT('',#10687);
#1804=VERTEX_POINT('',#11193);
#1805=VERTEX_POINT('',#11194);
#1806=VERTEX_POINT('',#11677);
#1807=VERTEX_POINT('',#11678);
#1808=VERTEX_POINT('',#11917);
#1809=VERTEX_POINT('',#11918);
#1810=VERTEX_POINT('',#12150);
#1811=VERTEX_POINT('',#12151);
#1812=VERTEX_POINT('',#12561);
#1813=VERTEX_POINT('',#12562);
#1814=VERTEX_POINT('',#13023);
#1815=VERTEX_POINT('',#13024);
#1816=VERTEX_POINT('',#13523);
#1817=VERTEX_POINT('',#13524);
#1818=VERTEX_POINT('',#13936);
#1819=VERTEX_POINT('',#13937);
#1820=VERTEX_POINT('',#14167);
#1821=VERTEX_POINT('',#14168);
#1822=VERTEX_POINT('',#14397);
#1823=VERTEX_POINT('',#14398);
#1824=VERTEX_POINT('',#14405);
#1825=VERTEX_POINT('',#14407);
#1826=VERTEX_POINT('',#14413);
#1827=VERTEX_POINT('',#14604);
#1828=VERTEX_POINT('',#14798);
#1829=VERTEX_POINT('',#14989);
#1830=VERTEX_POINT('',#15180);
#1831=VERTEX_POINT('',#15191);
#1832=VERTEX_POINT('',#15202);
#1833=VERTEX_POINT('',#15214);
#1834=VERTEX_POINT('',#15408);
#1835=VERTEX_POINT('',#15599);
#1836=VERTEX_POINT('',#15790);
#1837=VERTEX_POINT('',#15981);
#1838=VERTEX_POINT('',#15992);
#1839=VERTEX_POINT('',#16004);
#1840=VERTEX_POINT('',#16015);
#1841=VERTEX_POINT('',#16209);
#1842=VERTEX_POINT('',#16400);
#1843=VERTEX_POINT('',#16591);
#1844=VERTEX_POINT('',#16602);
#1845=VERTEX_POINT('',#16613);
#1846=VERTEX_POINT('',#16626);
#1847=VERTEX_POINT('',#16820);
#1848=VERTEX_POINT('',#17011);
#1849=VERTEX_POINT('',#17018);
#1850=VERTEX_POINT('',#17020);
#1851=VERTEX_POINT('',#17026);
#1852=VERTEX_POINT('',#17217);
#1853=VERTEX_POINT('',#17411);
#1854=VERTEX_POINT('',#17602);
#1855=VERTEX_POINT('',#17793);
#1856=VERTEX_POINT('',#17804);
#1857=VERTEX_POINT('',#17815);
#1858=VERTEX_POINT('',#17827);
#1859=VERTEX_POINT('',#18021);
#1860=VERTEX_POINT('',#18212);
#1861=VERTEX_POINT('',#18403);
#1862=VERTEX_POINT('',#18594);
#1863=VERTEX_POINT('',#18605);
#1864=VERTEX_POINT('',#18617);
#1865=VERTEX_POINT('',#18628);
#1866=VERTEX_POINT('',#18822);
#1867=VERTEX_POINT('',#19013);
#1868=VERTEX_POINT('',#19204);
#1869=VERTEX_POINT('',#19215);
#1870=VERTEX_POINT('',#19226);
#1871=VERTEX_POINT('',#19238);
#1872=VERTEX_POINT('',#19623);
#1873=VERTEX_POINT('',#19824);
#1874=VERTEX_POINT('',#20626);
#1875=VERTEX_POINT('',#21304);
#1876=VERTEX_POINT('',#21493);
#1877=VERTEX_POINT('',#21496);
#1878=VERTEX_POINT('',#21500);
#1879=VERTEX_POINT('',#21506);
#1880=VERTEX_POINT('',#21508);
#1881=VERTEX_POINT('',#21512);
#1882=VERTEX_POINT('',#21513);
#1883=VERTEX_POINT('',#21515);
#1884=VERTEX_POINT('',#21517);
#1885=VERTEX_POINT('',#21521);
#1886=VERTEX_POINT('',#21523);
#1887=VERTEX_POINT('',#21527);
#1888=VERTEX_POINT('',#21529);
#1889=VERTEX_POINT('',#21533);
#1890=VERTEX_POINT('',#21535);
#1891=VERTEX_POINT('',#21539);
#1892=VERTEX_POINT('',#21541);
#1893=VERTEX_POINT('',#21551);
#1894=VERTEX_POINT('',#21552);
#1895=VERTEX_POINT('',#21563);
#1896=VERTEX_POINT('',#21565);
#1897=VERTEX_POINT('',#21569);
#1898=VERTEX_POINT('',#21570);
#1899=VERTEX_POINT('',#21586);
#1900=VERTEX_POINT('',#21588);
#1901=VERTEX_POINT('',#21592);
#1902=VERTEX_POINT('',#21596);
#1903=VERTEX_POINT('',#21598);
#1904=VERTEX_POINT('',#21600);
#1905=VERTEX_POINT('',#21602);
#1906=VERTEX_POINT('',#21604);
#1907=VERTEX_POINT('',#21619);
#1908=VERTEX_POINT('',#21630);
#1909=VERTEX_POINT('',#21636);
#1910=VERTEX_POINT('',#21638);
#1911=VERTEX_POINT('',#21640);
#1912=VERTEX_POINT('',#21642);
#1913=VERTEX_POINT('',#21644);
#1914=VERTEX_POINT('',#21701);
#1915=VERTEX_POINT('',#21703);
#1916=VERTEX_POINT('',#21706);
#1917=VERTEX_POINT('',#21709);
#1918=VERTEX_POINT('',#21714);
#1919=VERTEX_POINT('',#21717);
#1920=VERTEX_POINT('',#21722);
#1921=VERTEX_POINT('',#21725);
#1922=VERTEX_POINT('',#21727);
#1923=VERTEX_POINT('',#21732);
#1924=VERTEX_POINT('',#21735);
#1925=VERTEX_POINT('',#21737);
#1926=VERTEX_POINT('',#21742);
#1927=VERTEX_POINT('',#21746);
#1928=VERTEX_POINT('',#21750);
#1929=VERTEX_POINT('',#21752);
#1930=VERTEX_POINT('',#21865);
#1931=VERTEX_POINT('',#21866);
#1932=VERTEX_POINT('',#21922);
#1933=VERTEX_POINT('',#21924);
#1934=VERTEX_POINT('',#21982);
#1935=VERTEX_POINT('',#21984);
#1936=VERTEX_POINT('',#21988);
#1937=VERTEX_POINT('',#21990);
#1938=VERTEX_POINT('',#21999);
#1939=VERTEX_POINT('',#22001);
#1940=VERTEX_POINT('',#22003);
#1941=VERTEX_POINT('',#22007);
#1942=VERTEX_POINT('',#22011);
#1943=VERTEX_POINT('',#22015);
#1944=VERTEX_POINT('',#22019);
#1945=VERTEX_POINT('',#22021);
#1946=VERTEX_POINT('',#22077);
#1947=VERTEX_POINT('',#22079);
#1948=VERTEX_POINT('',#22081);
#1949=VERTEX_POINT('',#22084);
#1950=VERTEX_POINT('',#22086);
#1951=VERTEX_POINT('',#22253);
#1952=VERTEX_POINT('',#22254);
#1953=VERTEX_POINT('',#22275);
#1954=VERTEX_POINT('',#22277);
#1955=VERTEX_POINT('',#22331);
#1956=VERTEX_POINT('',#22332);
#1957=VERTEX_POINT('',#22334);
#1958=VERTEX_POINT('',#22351);
#1959=VERTEX_POINT('',#22366);
#1960=VERTEX_POINT('',#22367);
#1961=VERTEX_POINT('',#22369);
#1962=VERTEX_POINT('',#22371);
#1963=VERTEX_POINT('',#22393);
#1964=VERTEX_POINT('',#22395);
#1965=VERTEX_POINT('',#22397);
#1966=VERTEX_POINT('',#22400);
#1967=VERTEX_POINT('',#22402);
#1968=VERTEX_POINT('',#22405);
#1969=VERTEX_POINT('',#22407);
#1970=VERTEX_POINT('',#22411);
#1971=VERTEX_POINT('',#22412);
#1972=VERTEX_POINT('',#22414);
#1973=VERTEX_POINT('',#22416);
#1974=VERTEX_POINT('',#22454);
#1975=VERTEX_POINT('',#22467);
#1976=VERTEX_POINT('',#22486);
#1977=VERTEX_POINT('',#22488);
#1978=VERTEX_POINT('',#22490);
#1979=VERTEX_POINT('',#22511);
#1980=VERTEX_POINT('',#22514);
#1981=VERTEX_POINT('',#22516);
#1982=VERTEX_POINT('',#22559);
#1983=VERTEX_POINT('',#22582);
#1984=VERTEX_POINT('',#22586);
#1985=VERTEX_POINT('',#22590);
#1986=VERTEX_POINT('',#22592);
#1987=VERTEX_POINT('',#22596);
#1988=VERTEX_POINT('',#22600);
#1989=VERTEX_POINT('',#22602);
#1990=VERTEX_POINT('',#22604);
#1991=VERTEX_POINT('',#22626);
#1992=VERTEX_POINT('',#22628);
#1993=VERTEX_POINT('',#22632);
#1994=VERTEX_POINT('',#22636);
#1995=VERTEX_POINT('',#22729);
#1996=VERTEX_POINT('',#22730);
#1997=VERTEX_POINT('',#22732);
#1998=VERTEX_POINT('',#22773);
#1999=VERTEX_POINT('',#22775);
#2000=VERTEX_POINT('',#22819);
#2001=VERTEX_POINT('',#22820);
#2002=VERTEX_POINT('',#22822);
#2003=VERTEX_POINT('',#22863);
#2004=VERTEX_POINT('',#22865);
#2005=VERTEX_POINT('',#22874);
#2006=VERTEX_POINT('',#22875);
#2007=VERTEX_POINT('',#22909);
#2008=VERTEX_POINT('',#22910);
#2009=VERTEX_POINT('',#22925);
#2010=VERTEX_POINT('',#22926);
#2011=VERTEX_POINT('',#22955);
#2012=VERTEX_POINT('',#22956);
#2013=VERTEX_POINT('',#22975);
#2014=VERTEX_POINT('',#22977);
#2015=VERTEX_POINT('',#22979);
#2016=VERTEX_POINT('',#22992);
#2017=VERTEX_POINT('',#22996);
#2018=VERTEX_POINT('',#23000);
#2019=VERTEX_POINT('',#23004);
#2020=VERTEX_POINT('',#23006);
#2021=VERTEX_POINT('',#23064);
#2022=VERTEX_POINT('',#23065);
#2023=VERTEX_POINT('',#23075);
#2024=VERTEX_POINT('',#23077);
#2025=VERTEX_POINT('',#23106);
#2026=VERTEX_POINT('',#23113);
#2027=VERTEX_POINT('',#23127);
#2028=VERTEX_POINT('',#23129);
#2029=VERTEX_POINT('',#23172);
#2030=VERTEX_POINT('',#23268);
#2031=VERTEX_POINT('',#23277);
#2032=VERTEX_POINT('',#23435);
#2033=VERTEX_POINT('',#23439);
#2034=VERTEX_POINT('',#23443);
#2035=EDGE_CURVE('',#1628,#1628,#1453,.T.);
#2036=EDGE_CURVE('',#1628,#1629,#883,.T.);
#2037=EDGE_CURVE('',#1629,#1629,#1454,.T.);
#2038=EDGE_CURVE('',#1630,#1630,#1455,.T.);
#2039=EDGE_CURVE('',#1630,#1631,#884,.T.);
#2040=EDGE_CURVE('',#1631,#1631,#1456,.T.);
#2041=EDGE_CURVE('',#1632,#1633,#1457,.T.);
#2042=EDGE_CURVE('',#1633,#1634,#885,.T.);
#2043=EDGE_CURVE('',#1635,#1634,#1458,.T.);
#2044=EDGE_CURVE('',#1632,#1635,#886,.T.);
#2045=EDGE_CURVE('',#1636,#1632,#887,.T.);
#2046=EDGE_CURVE('',#1637,#1635,#888,.T.);
#2047=EDGE_CURVE('',#1636,#1637,#889,.T.);
#2048=EDGE_CURVE('',#1638,#1636,#1459,.T.);
#2049=EDGE_CURVE('',#1639,#1637,#1460,.T.);
#2050=EDGE_CURVE('',#1638,#1639,#890,.T.);
#2051=EDGE_CURVE('',#1633,#1638,#891,.T.);
#2052=EDGE_CURVE('',#1634,#1639,#892,.T.);
#2053=EDGE_CURVE('',#1640,#1640,#1461,.T.);
#2054=EDGE_CURVE('',#1640,#1641,#1462,.T.);
#2055=EDGE_CURVE('',#1641,#1641,#1463,.T.);
#2056=EDGE_CURVE('',#1642,#1642,#1464,.T.);
#2057=EDGE_CURVE('',#1642,#1643,#1465,.T.);
#2058=EDGE_CURVE('',#1643,#1643,#1466,.T.);
#2059=EDGE_CURVE('',#1644,#1645,#207,.F.);
#2060=EDGE_CURVE('',#1644,#1646,#893,.T.);
#2061=EDGE_CURVE('',#1646,#1647,#208,.T.);
#2062=EDGE_CURVE('',#1647,#1645,#894,.T.);
#2063=EDGE_CURVE('',#1647,#1648,#895,.T.);
#2064=EDGE_CURVE('',#1649,#1648,#1467,.T.);
#2065=EDGE_CURVE('',#1650,#1649,#896,.T.);
#2066=EDGE_CURVE('',#1651,#1650,#1468,.T.);
#2067=EDGE_CURVE('',#1651,#1652,#897,.T.);
#2068=EDGE_CURVE('',#1652,#1653,#1469,.T.);
#2069=EDGE_CURVE('',#1653,#1654,#1470,.T.);
#2070=EDGE_CURVE('',#1654,#1655,#1471,.T.);
#2071=EDGE_CURVE('',#1655,#1656,#898,.T.);
#2072=EDGE_CURVE('',#1657,#1656,#1472,.T.);
#2073=EDGE_CURVE('',#1658,#1657,#899,.T.);
#2074=EDGE_CURVE('',#1659,#1658,#1473,.T.);
#2075=EDGE_CURVE('',#1659,#1645,#900,.T.);
#2076=EDGE_CURVE('',#1650,#1660,#901,.T.);
#2077=EDGE_CURVE('',#1660,#1661,#1474,.T.);
#2078=EDGE_CURVE('',#1661,#1651,#902,.T.);
#2079=EDGE_CURVE('',#1662,#1649,#903,.T.);
#2080=EDGE_CURVE('',#1662,#1660,#904,.T.);
#2081=EDGE_CURVE('',#1663,#1664,#1475,.T.);
#2082=EDGE_CURVE('',#1664,#1657,#905,.T.);
#2083=EDGE_CURVE('',#1656,#1663,#906,.T.);
#2084=EDGE_CURVE('',#1655,#1665,#907,.T.);
#2085=EDGE_CURVE('',#1663,#1665,#908,.T.);
#2086=EDGE_CURVE('',#1666,#1662,#1476,.T.);
#2087=EDGE_CURVE('',#1648,#1666,#909,.T.);
#2088=EDGE_CURVE('',#1646,#1667,#910,.T.);
#2089=EDGE_CURVE('',#1666,#1667,#911,.T.);
#2090=EDGE_CURVE('',#1658,#1668,#912,.T.);
#2091=EDGE_CURVE('',#1668,#1669,#1477,.T.);
#2092=EDGE_CURVE('',#1669,#1659,#913,.T.);
#2093=EDGE_CURVE('',#1670,#1669,#914,.T.);
#2094=EDGE_CURVE('',#1670,#1644,#915,.T.);
#2095=EDGE_CURVE('',#1671,#1672,#1478,.T.);
#2096=EDGE_CURVE('',#1653,#1671,#916,.T.);
#2097=EDGE_CURVE('',#1652,#1672,#917,.T.);
#2098=EDGE_CURVE('',#1672,#1661,#918,.T.);
#2099=EDGE_CURVE('',#1665,#1673,#1479,.T.);
#2100=EDGE_CURVE('',#1654,#1673,#919,.T.);
#2101=EDGE_CURVE('',#1673,#1671,#1480,.T.);
#2102=EDGE_CURVE('',#1674,#1646,#920,.T.);
#2103=EDGE_CURVE('',#1675,#1674,#921,.T.);
#2104=EDGE_CURVE('',#1676,#1675,#922,.T.);
#2105=EDGE_CURVE('',#1676,#1667,#923,.T.);
#2106=EDGE_CURVE('',#1676,#1677,#924,.T.);
#2107=EDGE_CURVE('',#1677,#1670,#925,.T.);
#2108=EDGE_CURVE('',#1664,#1668,#926,.T.);
#2109=EDGE_CURVE('',#1678,#1679,#927,.T.);
#2110=EDGE_CURVE('',#1679,#1680,#928,.T.);
#2111=EDGE_CURVE('',#1681,#1680,#929,.T.);
#2112=EDGE_CURVE('',#1678,#1681,#930,.T.);
#2113=EDGE_CURVE('',#1682,#1678,#1481,.T.);
#2114=EDGE_CURVE('',#1683,#1681,#1482,.T.);
#2115=EDGE_CURVE('',#1682,#1683,#931,.T.);
#2116=EDGE_CURVE('',#1684,#1682,#932,.T.);
#2117=EDGE_CURVE('',#1685,#1683,#933,.T.);
#2118=EDGE_CURVE('',#1684,#1685,#934,.T.);
#2119=EDGE_CURVE('',#1679,#1684,#1483,.T.);
#2120=EDGE_CURVE('',#1680,#1685,#1484,.T.);
#2121=EDGE_CURVE('',#1686,#1687,#935,.T.);
#2122=EDGE_CURVE('',#1687,#1688,#936,.T.);
#2123=EDGE_CURVE('',#1689,#1688,#937,.T.);
#2124=EDGE_CURVE('',#1686,#1689,#938,.T.);
#2125=EDGE_CURVE('',#1690,#1686,#1485,.T.);
#2126=EDGE_CURVE('',#1691,#1689,#1486,.T.);
#2127=EDGE_CURVE('',#1690,#1691,#939,.T.);
#2128=EDGE_CURVE('',#1692,#1690,#940,.T.);
#2129=EDGE_CURVE('',#1693,#1691,#941,.T.);
#2130=EDGE_CURVE('',#1692,#1693,#942,.T.);
#2131=EDGE_CURVE('',#1687,#1692,#1487,.T.);
#2132=EDGE_CURVE('',#1688,#1693,#1488,.T.);
#2133=EDGE_CURVE('',#1677,#1694,#943,.T.);
#2134=EDGE_CURVE('',#1694,#1695,#944,.T.);
#2135=EDGE_CURVE('',#1644,#1695,#945,.T.);
#2136=EDGE_CURVE('',#1696,#1675,#1489,.T.);
#2137=EDGE_CURVE('',#1697,#1674,#1490,.T.);
#2138=EDGE_CURVE('',#1696,#1697,#946,.T.);
#2139=EDGE_CURVE('',#1696,#1698,#947,.T.);
#2140=EDGE_CURVE('',#1699,#1697,#948,.T.);
#2141=EDGE_CURVE('',#1698,#1699,#949,.T.);
#2142=EDGE_CURVE('',#1694,#1698,#1491,.T.);
#2143=EDGE_CURVE('',#1695,#1699,#1492,.T.);
#2144=EDGE_CURVE('',#1700,#1700,#1493,.T.);
#2145=EDGE_CURVE('',#1700,#1701,#1494,.T.);
#2146=EDGE_CURVE('',#1701,#1701,#1495,.T.);
#2147=EDGE_CURVE('',#1702,#1702,#1496,.T.);
#2148=EDGE_CURVE('',#1702,#1703,#1497,.T.);
#2149=EDGE_CURVE('',#1703,#1703,#1498,.T.);
#2150=EDGE_CURVE('',#1704,#1705,#209,.T.);
#2151=EDGE_CURVE('',#1705,#1706,#950,.T.);
#2152=EDGE_CURVE('',#1707,#1706,#210,.F.);
#2153=EDGE_CURVE('',#1707,#1704,#951,.T.);
#2154=EDGE_CURVE('',#1708,#1707,#952,.T.);
#2155=EDGE_CURVE('',#1709,#1708,#1499,.T.);
#2156=EDGE_CURVE('',#1710,#1709,#953,.T.);
#2157=EDGE_CURVE('',#1711,#1710,#1500,.T.);
#2158=EDGE_CURVE('',#1704,#1711,#954,.T.);
#2159=EDGE_CURVE('',#1712,#1713,#1501,.T.);
#2160=EDGE_CURVE('',#1714,#1712,#955,.T.);
#2161=EDGE_CURVE('',#1715,#1714,#1502,.T.);
#2162=EDGE_CURVE('',#1713,#1715,#956,.T.);
#2163=EDGE_CURVE('',#1716,#1717,#1503,.T.);
#2164=EDGE_CURVE('',#1718,#1716,#957,.T.);
#2165=EDGE_CURVE('',#1719,#1718,#1504,.T.);
#2166=EDGE_CURVE('',#1717,#1719,#958,.T.);
#2167=EDGE_CURVE('',#1720,#1721,#1505,.T.);
#2168=EDGE_CURVE('',#1722,#1720,#959,.T.);
#2169=EDGE_CURVE('',#1723,#1722,#1506,.T.);
#2170=EDGE_CURVE('',#1721,#1723,#960,.T.);
#2171=EDGE_CURVE('',#1724,#1723,#961,.T.);
#2172=EDGE_CURVE('',#1724,#1725,#962,.T.);
#2173=EDGE_CURVE('',#1721,#1725,#963,.T.);
#2174=EDGE_CURVE('',#1726,#1705,#964,.T.);
#2175=EDGE_CURVE('',#1726,#1727,#1507,.T.);
#2176=EDGE_CURVE('',#1727,#1728,#965,.T.);
#2177=EDGE_CURVE('',#1728,#1729,#1508,.T.);
#2178=EDGE_CURVE('',#1730,#1729,#966,.T.);
#2179=EDGE_CURVE('',#1731,#1730,#1509,.T.);
#2180=EDGE_CURVE('',#1732,#1731,#1510,.T.);
#2181=EDGE_CURVE('',#1733,#1732,#1511,.T.);
#2182=EDGE_CURVE('',#1720,#1733,#967,.T.);
#2183=EDGE_CURVE('',#1725,#1734,#1512,.T.);
#2184=EDGE_CURVE('',#1706,#1734,#968,.T.);
#2185=EDGE_CURVE('',#1735,#1736,#1513,.T.);
#2186=EDGE_CURVE('',#1729,#1735,#969,.T.);
#2187=EDGE_CURVE('',#1736,#1728,#970,.T.);
#2188=EDGE_CURVE('',#1735,#1737,#971,.T.);
#2189=EDGE_CURVE('',#1730,#1737,#972,.T.);
#2190=EDGE_CURVE('',#1738,#1724,#1514,.T.);
#2191=EDGE_CURVE('',#1734,#1738,#973,.T.);
#2192=EDGE_CURVE('',#1738,#1739,#974,.T.);
#2193=EDGE_CURVE('',#1707,#1739,#975,.T.);
#2194=EDGE_CURVE('',#1740,#1726,#976,.T.);
#2195=EDGE_CURVE('',#1741,#1740,#1515,.T.);
#2196=EDGE_CURVE('',#1727,#1741,#977,.T.);
#2197=EDGE_CURVE('',#1704,#1742,#978,.T.);
#2198=EDGE_CURVE('',#1742,#1740,#979,.T.);
#2199=EDGE_CURVE('',#1743,#1744,#1516,.T.);
#2200=EDGE_CURVE('',#1733,#1744,#980,.T.);
#2201=EDGE_CURVE('',#1732,#1743,#981,.T.);
#2202=EDGE_CURVE('',#1744,#1722,#982,.T.);
#2203=EDGE_CURVE('',#1737,#1745,#1517,.T.);
#2204=EDGE_CURVE('',#1731,#1745,#983,.T.);
#2205=EDGE_CURVE('',#1745,#1743,#1518,.T.);
#2206=EDGE_CURVE('',#1746,#1739,#984,.T.);
#2207=EDGE_CURVE('',#1746,#1747,#985,.T.);
#2208=EDGE_CURVE('',#1747,#1708,#986,.T.);
#2209=EDGE_CURVE('',#1736,#1741,#987,.T.);
#2210=EDGE_CURVE('',#1748,#1742,#988,.T.);
#2211=EDGE_CURVE('',#1746,#1748,#989,.T.);
#2212=EDGE_CURVE('',#1749,#1750,#990,.T.);
#2213=EDGE_CURVE('',#1749,#1714,#991,.T.);
#2214=EDGE_CURVE('',#1750,#1712,#992,.T.);
#2215=EDGE_CURVE('',#1751,#1749,#1519,.T.);
#2216=EDGE_CURVE('',#1751,#1715,#993,.T.);
#2217=EDGE_CURVE('',#1752,#1751,#994,.T.);
#2218=EDGE_CURVE('',#1752,#1713,#995,.T.);
#2219=EDGE_CURVE('',#1750,#1752,#1520,.T.);
#2220=EDGE_CURVE('',#1753,#1754,#996,.T.);
#2221=EDGE_CURVE('',#1753,#1718,#997,.T.);
#2222=EDGE_CURVE('',#1754,#1716,#998,.T.);
#2223=EDGE_CURVE('',#1755,#1753,#1521,.T.);
#2224=EDGE_CURVE('',#1755,#1719,#999,.T.);
#2225=EDGE_CURVE('',#1756,#1755,#1000,.T.);
#2226=EDGE_CURVE('',#1756,#1717,#1001,.T.);
#2227=EDGE_CURVE('',#1754,#1756,#1522,.T.);
#2228=EDGE_CURVE('',#1757,#1711,#1002,.T.);
#2229=EDGE_CURVE('',#1748,#1757,#1003,.T.);
#2230=EDGE_CURVE('',#1758,#1747,#1523,.T.);
#2231=EDGE_CURVE('',#1758,#1709,#1004,.T.);
#2232=EDGE_CURVE('',#1758,#1759,#1005,.T.);
#2233=EDGE_CURVE('',#1759,#1710,#1006,.T.);
#2234=EDGE_CURVE('',#1757,#1759,#1524,.T.);
#2235=EDGE_CURVE('',#1760,#1760,#1525,.T.);
#2236=EDGE_CURVE('',#1760,#1761,#1007,.T.);
#2237=EDGE_CURVE('',#1761,#1761,#1526,.T.);
#2238=EDGE_CURVE('',#1762,#1763,#1008,.T.);
#2239=EDGE_CURVE('',#1762,#1764,#1009,.T.);
#2240=EDGE_CURVE('',#1765,#1764,#1010,.T.);
#2241=EDGE_CURVE('',#1763,#1765,#1011,.T.);
#2242=EDGE_CURVE('',#1763,#1766,#1012,.T.);
#2243=EDGE_CURVE('',#1767,#1765,#1013,.T.);
#2244=EDGE_CURVE('',#1766,#1767,#1014,.T.);
#2245=EDGE_CURVE('',#1766,#1768,#1015,.T.);
#2246=EDGE_CURVE('',#1769,#1767,#1016,.T.);
#2247=EDGE_CURVE('',#1768,#1769,#1017,.T.);
#2248=EDGE_CURVE('',#1768,#1770,#1018,.T.);
#2249=EDGE_CURVE('',#1771,#1769,#1019,.T.);
#2250=EDGE_CURVE('',#1770,#1771,#1020,.T.);
#2251=EDGE_CURVE('',#1770,#1772,#1021,.T.);
#2252=EDGE_CURVE('',#1773,#1771,#1022,.T.);
#2253=EDGE_CURVE('',#1772,#1773,#1023,.T.);
#2254=EDGE_CURVE('',#1772,#1762,#1024,.T.);
#2255=EDGE_CURVE('',#1764,#1773,#1025,.T.);
#2256=EDGE_CURVE('',#1774,#1775,#1026,.T.);
#2257=EDGE_CURVE('',#1776,#1774,#71,.F.);
#2258=EDGE_CURVE('',#1777,#1776,#1527,.T.);
#2259=EDGE_CURVE('',#1777,#1775,#72,.T.);
#2260=EDGE_CURVE('',#1778,#1779,#1027,.T.);
#2261=EDGE_CURVE('',#1774,#1778,#73,.F.);
#2262=EDGE_CURVE('',#1775,#1779,#74,.T.);
#2263=EDGE_CURVE('',#1780,#1781,#1028,.T.);
#2264=EDGE_CURVE('',#1778,#1780,#75,.T.);
#2265=EDGE_CURVE('',#1779,#1781,#76,.T.);
#2266=EDGE_CURVE('',#1782,#1783,#1029,.T.);
#2267=EDGE_CURVE('',#1780,#1782,#77,.T.);
#2268=EDGE_CURVE('',#1781,#1783,#78,.T.);
#2269=EDGE_CURVE('',#1784,#1785,#1030,.T.);
#2270=EDGE_CURVE('',#1782,#1784,#79,.F.);
#2271=EDGE_CURVE('',#1783,#1785,#80,.T.);
#2272=EDGE_CURVE('',#1786,#1787,#1031,.T.);
#2273=EDGE_CURVE('',#1784,#1786,#81,.F.);
#2274=EDGE_CURVE('',#1785,#1787,#82,.T.);
#2275=EDGE_CURVE('',#1788,#1789,#1032,.T.);
#2276=EDGE_CURVE('',#1786,#1788,#83,.F.);
#2277=EDGE_CURVE('',#1787,#1789,#84,.T.);
#2278=EDGE_CURVE('',#1790,#1791,#1033,.T.);
#2279=EDGE_CURVE('',#1788,#1790,#85,.F.);
#2280=EDGE_CURVE('',#1789,#1791,#86,.T.);
#2281=EDGE_CURVE('',#1792,#1793,#1034,.T.);
#2282=EDGE_CURVE('',#1790,#1792,#87,.T.);
#2283=EDGE_CURVE('',#1791,#1793,#88,.T.);
#2284=EDGE_CURVE('',#1794,#1795,#1035,.T.);
#2285=EDGE_CURVE('',#1792,#1794,#89,.F.);
#2286=EDGE_CURVE('',#1793,#1795,#90,.T.);
#2287=EDGE_CURVE('',#1796,#1797,#1036,.T.);
#2288=EDGE_CURVE('',#1794,#1796,#91,.F.);
#2289=EDGE_CURVE('',#1795,#1798,#92,.T.);
#2290=EDGE_CURVE('',#1798,#1797,#93,.T.);
#2291=EDGE_CURVE('',#1799,#1800,#1037,.T.);
#2292=EDGE_CURVE('',#1796,#1799,#94,.F.);
#2293=EDGE_CURVE('',#1797,#1800,#95,.T.);
#2294=EDGE_CURVE('',#1801,#1802,#1038,.T.);
#2295=EDGE_CURVE('',#1803,#1801,#96,.F.);
#2296=EDGE_CURVE('',#1799,#1803,#97,.F.);
#2297=EDGE_CURVE('',#1800,#1802,#98,.T.);
#2298=EDGE_CURVE('',#1804,#1805,#1039,.T.);
#2299=EDGE_CURVE('',#1801,#1804,#99,.F.);
#2300=EDGE_CURVE('',#1802,#1805,#100,.T.);
#2301=EDGE_CURVE('',#1806,#1807,#1040,.T.);
#2302=EDGE_CURVE('',#1804,#1806,#101,.F.);
#2303=EDGE_CURVE('',#1805,#1807,#102,.T.);
#2304=EDGE_CURVE('',#1808,#1809,#1041,.T.);
#2305=EDGE_CURVE('',#1806,#1808,#103,.T.);
#2306=EDGE_CURVE('',#1807,#1809,#104,.T.);
#2307=EDGE_CURVE('',#1810,#1811,#1042,.T.);
#2308=EDGE_CURVE('',#1808,#1810,#105,.T.);
#2309=EDGE_CURVE('',#1809,#1811,#106,.T.);
#2310=EDGE_CURVE('',#1812,#1813,#1043,.T.);
#2311=EDGE_CURVE('',#1810,#1812,#107,.F.);
#2312=EDGE_CURVE('',#1811,#1813,#108,.T.);
#2313=EDGE_CURVE('',#1814,#1815,#1044,.T.);
#2314=EDGE_CURVE('',#1812,#1814,#109,.F.);
#2315=EDGE_CURVE('',#1813,#1815,#110,.T.);
#2316=EDGE_CURVE('',#1816,#1817,#1045,.T.);
#2317=EDGE_CURVE('',#1814,#1816,#111,.F.);
#2318=EDGE_CURVE('',#1815,#1817,#112,.T.);
#2319=EDGE_CURVE('',#1818,#1819,#1046,.T.);
#2320=EDGE_CURVE('',#1816,#1818,#113,.F.);
#2321=EDGE_CURVE('',#1817,#1819,#114,.T.);
#2322=EDGE_CURVE('',#1820,#1821,#1047,.T.);
#2323=EDGE_CURVE('',#1818,#1820,#115,.T.);
#2324=EDGE_CURVE('',#1819,#1821,#116,.F.);
#2325=EDGE_CURVE('',#1822,#1823,#117,.T.);
#2326=EDGE_CURVE('',#1824,#1823,#1528,.T.);
#2327=EDGE_CURVE('',#1824,#1825,#118,.T.);
#2328=EDGE_CURVE('',#1825,#1826,#119,.T.);
#2329=EDGE_CURVE('',#1826,#1827,#120,.T.);
#2330=EDGE_CURVE('',#1827,#1828,#121,.T.);
#2331=EDGE_CURVE('',#1828,#1829,#122,.T.);
#2332=EDGE_CURVE('',#1829,#1830,#123,.T.);
#2333=EDGE_CURVE('',#1830,#1831,#124,.T.);
#2334=EDGE_CURVE('',#1831,#1832,#125,.T.);
#2335=EDGE_CURVE('',#1832,#1833,#126,.T.);
#2336=EDGE_CURVE('',#1833,#1834,#127,.T.);
#2337=EDGE_CURVE('',#1834,#1835,#128,.T.);
#2338=EDGE_CURVE('',#1835,#1836,#129,.T.);
#2339=EDGE_CURVE('',#1836,#1837,#130,.T.);
#2340=EDGE_CURVE('',#1837,#1838,#131,.T.);
#2341=EDGE_CURVE('',#1838,#1839,#132,.T.);
#2342=EDGE_CURVE('',#1839,#1840,#133,.T.);
#2343=EDGE_CURVE('',#1840,#1841,#134,.T.);
#2344=EDGE_CURVE('',#1841,#1842,#135,.T.);
#2345=EDGE_CURVE('',#1842,#1843,#136,.T.);
#2346=EDGE_CURVE('',#1843,#1844,#137,.T.);
#2347=EDGE_CURVE('',#1844,#1845,#138,.T.);
#2348=EDGE_CURVE('',#1845,#1846,#139,.T.);
#2349=EDGE_CURVE('',#1846,#1847,#140,.T.);
#2350=EDGE_CURVE('',#1847,#1848,#141,.T.);
#2351=EDGE_CURVE('',#1849,#1848,#1529,.F.);
#2352=EDGE_CURVE('',#1849,#1850,#142,.T.);
#2353=EDGE_CURVE('',#1850,#1851,#143,.T.);
#2354=EDGE_CURVE('',#1851,#1852,#144,.T.);
#2355=EDGE_CURVE('',#1852,#1853,#145,.T.);
#2356=EDGE_CURVE('',#1853,#1854,#146,.T.);
#2357=EDGE_CURVE('',#1854,#1855,#147,.T.);
#2358=EDGE_CURVE('',#1855,#1856,#148,.T.);
#2359=EDGE_CURVE('',#1856,#1857,#149,.T.);
#2360=EDGE_CURVE('',#1857,#1858,#150,.T.);
#2361=EDGE_CURVE('',#1858,#1859,#151,.T.);
#2362=EDGE_CURVE('',#1859,#1860,#152,.T.);
#2363=EDGE_CURVE('',#1860,#1861,#153,.T.);
#2364=EDGE_CURVE('',#1861,#1862,#154,.T.);
#2365=EDGE_CURVE('',#1862,#1863,#155,.T.);
#2366=EDGE_CURVE('',#1863,#1864,#156,.T.);
#2367=EDGE_CURVE('',#1864,#1865,#157,.T.);
#2368=EDGE_CURVE('',#1865,#1866,#158,.T.);
#2369=EDGE_CURVE('',#1866,#1867,#159,.T.);
#2370=EDGE_CURVE('',#1867,#1868,#160,.T.);
#2371=EDGE_CURVE('',#1868,#1869,#161,.T.);
#2372=EDGE_CURVE('',#1869,#1870,#162,.T.);
#2373=EDGE_CURVE('',#1870,#1871,#163,.T.);
#2374=EDGE_CURVE('',#1871,#1822,#164,.T.);
#2375=EDGE_CURVE('',#1821,#1872,#165,.F.);
#2376=EDGE_CURVE('',#1873,#1872,#1530,.T.);
#2377=EDGE_CURVE('',#1820,#1873,#166,.T.);
#2378=EDGE_CURVE('',#1848,#1873,#167,.T.);
#2379=EDGE_CURVE('',#1874,#1824,#168,.T.);
#2380=EDGE_CURVE('',#1874,#1776,#169,.T.);
#2381=EDGE_CURVE('',#1875,#1849,#170,.T.);
#2382=EDGE_CURVE('',#1872,#1875,#171,.T.);
#2383=EDGE_CURVE('',#1823,#1777,#172,.T.);
#2384=EDGE_CURVE('',#1876,#1876,#1531,.T.);
#2385=EDGE_CURVE('',#1877,#1877,#1532,.T.);
#2386=EDGE_CURVE('',#1877,#1876,#1048,.T.);
#2387=EDGE_CURVE('',#1877,#1878,#1049,.T.);
#2388=EDGE_CURVE('',#1878,#1878,#1533,.T.);
#2389=EDGE_CURVE('',#1879,#1879,#1534,.T.);
#2390=EDGE_CURVE('',#1879,#1880,#1050,.T.);
#2391=EDGE_CURVE('',#1880,#1880,#1535,.T.);
#2392=EDGE_CURVE('',#1881,#1882,#1051,.T.);
#2393=EDGE_CURVE('',#1881,#1883,#1052,.T.);
#2394=EDGE_CURVE('',#1884,#1883,#1053,.T.);
#2395=EDGE_CURVE('',#1882,#1884,#1054,.T.);
#2396=EDGE_CURVE('',#1882,#1885,#1055,.T.);
#2397=EDGE_CURVE('',#1886,#1884,#1056,.T.);
#2398=EDGE_CURVE('',#1885,#1886,#1057,.T.);
#2399=EDGE_CURVE('',#1885,#1887,#1058,.T.);
#2400=EDGE_CURVE('',#1888,#1886,#1059,.T.);
#2401=EDGE_CURVE('',#1887,#1888,#1060,.T.);
#2402=EDGE_CURVE('',#1887,#1889,#1061,.T.);
#2403=EDGE_CURVE('',#1890,#1888,#1062,.T.);
#2404=EDGE_CURVE('',#1889,#1890,#1063,.T.);
#2405=EDGE_CURVE('',#1889,#1891,#1064,.T.);
#2406=EDGE_CURVE('',#1892,#1890,#1065,.T.);
#2407=EDGE_CURVE('',#1891,#1892,#1066,.T.);
#2408=EDGE_CURVE('',#1891,#1881,#1067,.T.);
#2409=EDGE_CURVE('',#1883,#1892,#1068,.T.);
#2410=EDGE_CURVE('',#1893,#1894,#173,.T.);
#2411=EDGE_CURVE('',#1894,#1895,#1536,.T.);
#2412=EDGE_CURVE('',#1895,#1896,#1537,.T.);
#2413=EDGE_CURVE('',#1896,#1893,#1538,.T.);
#2414=EDGE_CURVE('',#1897,#1898,#174,.T.);
#2415=EDGE_CURVE('',#1898,#1896,#1539,.T.);
#2416=EDGE_CURVE('',#1895,#1897,#1540,.T.);
#2417=EDGE_CURVE('',#1896,#1899,#1069,.T.);
#2418=EDGE_CURVE('',#1900,#1899,#1541,.T.);
#2419=EDGE_CURVE('',#1893,#1900,#1070,.T.);
#2420=EDGE_CURVE('',#1898,#1901,#1071,.T.);
#2421=EDGE_CURVE('',#1899,#1901,#1542,.T.);
#2422=EDGE_CURVE('',#1897,#1902,#1543,.T.);
#2423=EDGE_CURVE('',#1903,#1902,#1072,.T.);
#2424=EDGE_CURVE('',#1904,#1903,#1073,.T.);
#2425=EDGE_CURVE('',#1904,#1905,#1074,.T.);
#2426=EDGE_CURVE('',#1906,#1905,#1544,.T.);
#2427=EDGE_CURVE('',#1901,#1906,#175,.T.);
#2428=EDGE_CURVE('',#1907,#1900,#176,.T.);
#2429=EDGE_CURVE('',#1899,#1908,#1545,.T.);
#2430=EDGE_CURVE('',#1908,#1907,#1546,.T.);
#2431=EDGE_CURVE('',#1906,#1908,#1547,.T.);
#2432=EDGE_CURVE('',#1905,#1909,#1075,.T.);
#2433=EDGE_CURVE('',#1909,#1910,#1548,.T.);
#2434=EDGE_CURVE('',#1910,#1911,#1549,.T.);
#2435=EDGE_CURVE('',#1911,#1912,#1550,.T.);
#2436=EDGE_CURVE('',#1912,#1913,#177,.T.);
#2437=EDGE_CURVE('',#1913,#1907,#1076,.T.);
#2438=EDGE_CURVE('',#1914,#1914,#1551,.T.);
#2439=EDGE_CURVE('',#1915,#1915,#1552,.T.);
#2440=EDGE_CURVE('',#1916,#1916,#1553,.T.);
#2441=EDGE_CURVE('',#1917,#1917,#1554,.T.);
#2442=EDGE_CURVE('',#1917,#1915,#1555,.T.);
#2443=EDGE_CURVE('',#1918,#1918,#1556,.T.);
#2444=EDGE_CURVE('',#1919,#1919,#1557,.T.);
#2445=EDGE_CURVE('',#1919,#1914,#1558,.T.);
#2446=EDGE_CURVE('',#1920,#1920,#1559,.T.);
#2447=EDGE_CURVE('',#1921,#1921,#1560,.T.);
#2448=EDGE_CURVE('',#1921,#1922,#1561,.T.);
#2449=EDGE_CURVE('',#1922,#1922,#1562,.T.);
#2450=EDGE_CURVE('',#1923,#1923,#1563,.T.);
#2451=EDGE_CURVE('',#1924,#1924,#1564,.T.);
#2452=EDGE_CURVE('',#1924,#1925,#1565,.T.);
#2453=EDGE_CURVE('',#1925,#1925,#1566,.T.);
#2454=EDGE_CURVE('',#1923,#1926,#1077,.T.);
#2455=EDGE_CURVE('',#1926,#1926,#1567,.T.);
#2456=EDGE_CURVE('',#1920,#1927,#1078,.T.);
#2457=EDGE_CURVE('',#1927,#1927,#1568,.T.);
#2458=EDGE_CURVE('',#1928,#1903,#1079,.T.);
#2459=EDGE_CURVE('',#1902,#1929,#1080,.T.);
#2460=EDGE_CURVE('',#1928,#1929,#1081,.T.);
#2461=EDGE_CURVE('',#1930,#1931,#178,.T.);
#2462=EDGE_CURVE('',#1930,#1932,#1082,.T.);
#2463=EDGE_CURVE('',#1932,#1933,#179,.T.);
#2464=EDGE_CURVE('',#1931,#1933,#1083,.T.);
#2465=EDGE_CURVE('',#1934,#1930,#1569,.T.);
#2466=EDGE_CURVE('',#1934,#1935,#1084,.T.);
#2467=EDGE_CURVE('',#1935,#1932,#1570,.T.);
#2468=EDGE_CURVE('',#1934,#1936,#1571,.T.);
#2469=EDGE_CURVE('',#1936,#1937,#1085,.T.);
#2470=EDGE_CURVE('',#1937,#1935,#1572,.T.);
#2471=EDGE_CURVE('',#1928,#1936,#1573,.T.);
#2472=EDGE_CURVE('',#1929,#1937,#1574,.T.);
#2473=EDGE_CURVE('',#1933,#1894,#1086,.T.);
#2474=EDGE_CURVE('',#1903,#1938,#1087,.T.);
#2475=EDGE_CURVE('',#1939,#1931,#1088,.T.);
#2476=EDGE_CURVE('',#1940,#1939,#1575,.T.);
#2477=EDGE_CURVE('',#1938,#1940,#1576,.T.);
#2478=EDGE_CURVE('',#1941,#1938,#1089,.T.);
#2479=EDGE_CURVE('',#1904,#1941,#1090,.T.);
#2480=EDGE_CURVE('',#1942,#1940,#1091,.T.);
#2481=EDGE_CURVE('',#1941,#1942,#1577,.T.);
#2482=EDGE_CURVE('',#1943,#1939,#1092,.T.);
#2483=EDGE_CURVE('',#1942,#1943,#1578,.T.);
#2484=EDGE_CURVE('',#1943,#1944,#1093,.T.);
#2485=EDGE_CURVE('',#1945,#1944,#180,.T.);
#2486=EDGE_CURVE('',#1946,#1945,#1579,.T.);
#2487=EDGE_CURVE('',#1946,#1947,#1580,.T.);
#2488=EDGE_CURVE('',#1948,#1947,#1581,.T.);
#2489=EDGE_CURVE('',#1948,#1904,#1094,.T.);
#2490=EDGE_CURVE('',#1949,#1949,#1582,.T.);
#2491=EDGE_CURVE('',#1950,#1950,#1583,.T.);
#2492=EDGE_CURVE('',#1949,#1918,#1095,.T.);
#2493=EDGE_CURVE('',#1950,#1916,#1096,.T.);
#2494=EDGE_CURVE('',#1948,#1909,#1097,.T.);
#2495=EDGE_CURVE('',#1944,#1913,#1098,.T.);
#2496=EDGE_CURVE('',#1945,#1912,#1099,.T.);
#2497=EDGE_CURVE('',#1946,#1911,#1100,.T.);
#2498=EDGE_CURVE('',#1947,#1910,#1101,.T.);
#2499=EDGE_CURVE('',#1951,#1952,#181,.T.);
#2500=EDGE_CURVE('',#1951,#1953,#1102,.T.);
#2501=EDGE_CURVE('',#1954,#1953,#182,.T.);
#2502=EDGE_CURVE('',#1952,#1954,#1103,.T.);
#2503=EDGE_CURVE('',#1955,#1956,#1104,.T.);
#2504=EDGE_CURVE('',#1957,#1955,#183,.T.);
#2505=EDGE_CURVE('',#1957,#1958,#1105,.T.);
#2506=EDGE_CURVE('',#1956,#1958,#184,.T.);
#2507=EDGE_CURVE('',#1959,#1960,#1584,.T.);
#2508=EDGE_CURVE('',#1959,#1961,#1106,.T.);
#2509=EDGE_CURVE('',#1962,#1961,#185,.T.);
#2510=EDGE_CURVE('',#1952,#1962,#1107,.T.);
#2511=EDGE_CURVE('',#1963,#1954,#1108,.T.);
#2512=EDGE_CURVE('',#1964,#1963,#1585,.T.);
#2513=EDGE_CURVE('',#1965,#1964,#1586,.T.);
#2514=EDGE_CURVE('',#1960,#1965,#1109,.T.);
#2515=EDGE_CURVE('',#1966,#1966,#1587,.T.);
#2516=EDGE_CURVE('',#1967,#1967,#1588,.T.);
#2517=EDGE_CURVE('',#1968,#1951,#1110,.T.);
#2518=EDGE_CURVE('',#1968,#1969,#1111,.T.);
#2519=EDGE_CURVE('',#1953,#1969,#1112,.T.);
#2520=EDGE_CURVE('',#1970,#1971,#1113,.T.);
#2521=EDGE_CURVE('',#1970,#1972,#1114,.T.);
#2522=EDGE_CURVE('',#1973,#1972,#1115,.T.);
#2523=EDGE_CURVE('',#1971,#1973,#1116,.T.);
#2524=EDGE_CURVE('',#1958,#1970,#1117,.T.);
#2525=EDGE_CURVE('',#1972,#1957,#1118,.T.);
#2526=EDGE_CURVE('',#1956,#1974,#186,.T.);
#2527=EDGE_CURVE('',#1975,#1974,#1119,.T.);
#2528=EDGE_CURVE('',#1975,#1955,#187,.T.);
#2529=EDGE_CURVE('',#1962,#1976,#1120,.T.);
#2530=EDGE_CURVE('',#1977,#1976,#1121,.T.);
#2531=EDGE_CURVE('',#1978,#1977,#188,.T.);
#2532=EDGE_CURVE('',#1979,#1978,#1122,.T.);
#2533=EDGE_CURVE('',#1968,#1979,#1589,.T.);
#2534=EDGE_CURVE('',#1971,#1980,#1590,.T.);
#2535=EDGE_CURVE('',#1981,#1980,#1123,.T.);
#2536=EDGE_CURVE('',#1974,#1981,#1124,.T.);
#2537=EDGE_CURVE('',#1982,#1961,#1125,.T.);
#2538=EDGE_CURVE('',#1976,#1982,#189,.T.);
#2539=EDGE_CURVE('',#1959,#1983,#1126,.T.);
#2540=EDGE_CURVE('',#1983,#1982,#1127,.T.);
#2541=EDGE_CURVE('',#1984,#1960,#1128,.T.);
#2542=EDGE_CURVE('',#1983,#1984,#1591,.T.);
#2543=EDGE_CURVE('',#1964,#1985,#1129,.T.);
#2544=EDGE_CURVE('',#1986,#1985,#1592,.T.);
#2545=EDGE_CURVE('',#1965,#1986,#1130,.T.);
#2546=EDGE_CURVE('',#1963,#1987,#1131,.T.);
#2547=EDGE_CURVE('',#1985,#1987,#1593,.T.);
#2548=EDGE_CURVE('',#1988,#1969,#1594,.T.);
#2549=EDGE_CURVE('',#1989,#1988,#1132,.T.);
#2550=EDGE_CURVE('',#1990,#1989,#190,.T.);
#2551=EDGE_CURVE('',#1987,#1990,#1133,.T.);
#2552=EDGE_CURVE('',#1991,#1975,#1134,.T.);
#2553=EDGE_CURVE('',#1992,#1991,#1135,.T.);
#2554=EDGE_CURVE('',#1992,#1973,#1595,.T.);
#2555=EDGE_CURVE('',#1993,#1993,#1596,.T.);
#2556=EDGE_CURVE('',#1993,#1966,#1136,.T.);
#2557=EDGE_CURVE('',#1994,#1994,#1597,.T.);
#2558=EDGE_CURVE('',#1994,#1967,#1137,.T.);
#2559=EDGE_CURVE('',#1984,#1986,#1138,.T.);
#2560=EDGE_CURVE('',#1977,#1990,#1139,.T.);
#2561=EDGE_CURVE('',#1978,#1989,#1140,.T.);
#2562=EDGE_CURVE('',#1979,#1988,#1141,.T.);
#2563=EDGE_CURVE('',#1980,#1992,#1142,.T.);
#2564=EDGE_CURVE('',#1981,#1991,#1143,.T.);
#2565=EDGE_CURVE('',#1995,#1996,#1598,.T.);
#2566=EDGE_CURVE('',#1996,#1997,#191,.T.);
#2567=EDGE_CURVE('',#1997,#1998,#1599,.T.);
#2568=EDGE_CURVE('',#1998,#1999,#192,.T.);
#2569=EDGE_CURVE('',#1999,#1995,#211,.T.);
#2570=EDGE_CURVE('',#2000,#2001,#1600,.T.);
#2571=EDGE_CURVE('',#2001,#2002,#193,.T.);
#2572=EDGE_CURVE('',#2002,#2003,#1601,.T.);
#2573=EDGE_CURVE('',#2003,#2004,#212,.T.);
#2574=EDGE_CURVE('',#2004,#2000,#194,.T.);
#2575=EDGE_CURVE('',#2005,#2006,#1602,.T.);
#2576=EDGE_CURVE('',#2006,#2001,#1144,.T.);
#2577=EDGE_CURVE('',#2000,#2005,#1145,.T.);
#2578=EDGE_CURVE('',#2007,#2008,#1603,.T.);
#2579=EDGE_CURVE('',#2008,#2006,#195,.T.);
#2580=EDGE_CURVE('',#2005,#2007,#196,.T.);
#2581=EDGE_CURVE('',#2009,#2010,#1604,.T.);
#2582=EDGE_CURVE('',#2010,#2008,#1146,.T.);
#2583=EDGE_CURVE('',#2007,#2009,#1147,.T.);
#2584=EDGE_CURVE('',#2011,#2012,#1605,.T.);
#2585=EDGE_CURVE('',#2012,#2010,#197,.T.);
#2586=EDGE_CURVE('',#2009,#2011,#198,.T.);
#2587=EDGE_CURVE('',#2011,#1998,#1148,.T.);
#2588=EDGE_CURVE('',#1997,#2012,#1149,.T.);
#2589=EDGE_CURVE('',#1995,#2003,#1150,.T.);
#2590=EDGE_CURVE('',#2002,#1996,#1151,.T.);
#2591=EDGE_CURVE('',#2013,#1997,#1606,.T.);
#2592=EDGE_CURVE('',#2014,#2013,#1152,.T.);
#2593=EDGE_CURVE('',#2015,#2014,#199,.T.);
#2594=EDGE_CURVE('',#2012,#2015,#1607,.T.);
#2595=EDGE_CURVE('',#1996,#2016,#1608,.T.);
#2596=EDGE_CURVE('',#2016,#2013,#1609,.T.);
#2597=EDGE_CURVE('',#2017,#2002,#1610,.T.);
#2598=EDGE_CURVE('',#2016,#2017,#1153,.T.);
#2599=EDGE_CURVE('',#2001,#2018,#1611,.T.);
#2600=EDGE_CURVE('',#2018,#2017,#1612,.T.);
#2601=EDGE_CURVE('',#2004,#2019,#1154,.T.);
#2602=EDGE_CURVE('',#2019,#2020,#1155,.T.);
#2603=EDGE_CURVE('',#1999,#2020,#1156,.T.);
#2604=EDGE_CURVE('',#2021,#2022,#200,.T.);
#2605=EDGE_CURVE('',#2022,#2023,#1613,.T.);
#2606=EDGE_CURVE('',#2023,#2024,#201,.T.);
#2607=EDGE_CURVE('',#2024,#2021,#202,.T.);
#2608=EDGE_CURVE('',#2022,#2025,#1614,.T.);
#2609=EDGE_CURVE('',#2025,#2023,#1615,.T.);
#2610=EDGE_CURVE('',#2008,#2021,#1616,.T.);
#2611=EDGE_CURVE('',#2024,#2006,#1617,.T.);
#2612=EDGE_CURVE('',#2025,#2026,#1157,.T.);
#2613=EDGE_CURVE('',#2018,#2026,#1618,.T.);
#2614=EDGE_CURVE('',#2018,#2023,#1158,.T.);
#2615=EDGE_CURVE('',#2022,#2027,#1159,.T.);
#2616=EDGE_CURVE('',#2028,#2027,#1619,.T.);
#2617=EDGE_CURVE('',#2028,#2025,#1160,.T.);
#2618=EDGE_CURVE('',#2029,#2021,#1161,.T.);
#2619=EDGE_CURVE('',#2027,#2029,#203,.T.);
#2620=EDGE_CURVE('',#2026,#2017,#1620,.T.);
#2621=EDGE_CURVE('',#2015,#2029,#204,.T.);
#2622=EDGE_CURVE('',#2029,#2010,#1621,.T.);
#2623=EDGE_CURVE('',#2014,#2027,#1622,.T.);
#2624=EDGE_CURVE('',#2014,#2028,#1623,.T.);
#2625=EDGE_CURVE('',#2030,#2013,#1624,.T.);
#2626=EDGE_CURVE('',#2030,#2028,#1162,.T.);
#2627=EDGE_CURVE('',#2016,#2030,#1625,.T.);
#2628=EDGE_CURVE('',#2026,#2030,#1163,.T.);
#2629=EDGE_CURVE('',#2031,#2020,#205,.T.);
#2630=EDGE_CURVE('',#2032,#2031,#1164,.T.);
#2631=EDGE_CURVE('',#1995,#2032,#1626,.T.);
#2632=EDGE_CURVE('',#2033,#2032,#1165,.T.);
#2633=EDGE_CURVE('',#2003,#2033,#1627,.T.);
#2634=EDGE_CURVE('',#2034,#2031,#1166,.T.);
#2635=EDGE_CURVE('',#2033,#2034,#1167,.T.);
#2636=EDGE_CURVE('',#2034,#2019,#206,.T.);
#2637=ORIENTED_EDGE('',*,*,#2035,.T.);
#2638=ORIENTED_EDGE('',*,*,#2036,.T.);
#2639=ORIENTED_EDGE('',*,*,#2037,.F.);
#2640=ORIENTED_EDGE('',*,*,#2036,.F.);
#2641=ORIENTED_EDGE('',*,*,#2038,.T.);
#2642=ORIENTED_EDGE('',*,*,#2039,.T.);
#2643=ORIENTED_EDGE('',*,*,#2040,.F.);
#2644=ORIENTED_EDGE('',*,*,#2039,.F.);
#2645=ORIENTED_EDGE('',*,*,#2041,.T.);
#2646=ORIENTED_EDGE('',*,*,#2042,.T.);
#2647=ORIENTED_EDGE('',*,*,#2043,.F.);
#2648=ORIENTED_EDGE('',*,*,#2044,.F.);
#2649=ORIENTED_EDGE('',*,*,#2045,.T.);
#2650=ORIENTED_EDGE('',*,*,#2044,.T.);
#2651=ORIENTED_EDGE('',*,*,#2046,.F.);
#2652=ORIENTED_EDGE('',*,*,#2047,.F.);
#2653=ORIENTED_EDGE('',*,*,#2048,.T.);
#2654=ORIENTED_EDGE('',*,*,#2047,.T.);
#2655=ORIENTED_EDGE('',*,*,#2049,.F.);
#2656=ORIENTED_EDGE('',*,*,#2050,.F.);
#2657=ORIENTED_EDGE('',*,*,#2051,.T.);
#2658=ORIENTED_EDGE('',*,*,#2050,.T.);
#2659=ORIENTED_EDGE('',*,*,#2052,.F.);
#2660=ORIENTED_EDGE('',*,*,#2042,.F.);
#2661=ORIENTED_EDGE('',*,*,#2052,.T.);
#2662=ORIENTED_EDGE('',*,*,#2049,.T.);
#2663=ORIENTED_EDGE('',*,*,#2046,.T.);
#2664=ORIENTED_EDGE('',*,*,#2043,.T.);
#2665=ORIENTED_EDGE('',*,*,#2040,.T.);
#2666=ORIENTED_EDGE('',*,*,#2037,.T.);
#2667=ORIENTED_EDGE('',*,*,#2051,.F.);
#2668=ORIENTED_EDGE('',*,*,#2041,.F.);
#2669=ORIENTED_EDGE('',*,*,#2045,.F.);
#2670=ORIENTED_EDGE('',*,*,#2048,.F.);
#2671=ORIENTED_EDGE('',*,*,#2038,.F.);
#2672=ORIENTED_EDGE('',*,*,#2035,.F.);
#2673=ORIENTED_EDGE('',*,*,#2053,.T.);
#2674=ORIENTED_EDGE('',*,*,#2054,.T.);
#2675=ORIENTED_EDGE('',*,*,#2055,.F.);
#2676=ORIENTED_EDGE('',*,*,#2054,.F.);
#2677=ORIENTED_EDGE('',*,*,#2053,.F.);
#2678=ORIENTED_EDGE('',*,*,#2056,.T.);
#2679=ORIENTED_EDGE('',*,*,#2057,.T.);
#2680=ORIENTED_EDGE('',*,*,#2058,.F.);
#2681=ORIENTED_EDGE('',*,*,#2057,.F.);
#2682=ORIENTED_EDGE('',*,*,#2056,.F.);
#2683=ORIENTED_EDGE('',*,*,#2059,.F.);
#2684=ORIENTED_EDGE('',*,*,#2060,.T.);
#2685=ORIENTED_EDGE('',*,*,#2061,.T.);
#2686=ORIENTED_EDGE('',*,*,#2062,.T.);
#2687=ORIENTED_EDGE('',*,*,#2062,.F.);
#2688=ORIENTED_EDGE('',*,*,#2063,.T.);
#2689=ORIENTED_EDGE('',*,*,#2064,.F.);
#2690=ORIENTED_EDGE('',*,*,#2065,.F.);
#2691=ORIENTED_EDGE('',*,*,#2066,.F.);
#2692=ORIENTED_EDGE('',*,*,#2067,.T.);
#2693=ORIENTED_EDGE('',*,*,#2068,.T.);
#2694=ORIENTED_EDGE('',*,*,#2069,.T.);
#2695=ORIENTED_EDGE('',*,*,#2070,.T.);
#2696=ORIENTED_EDGE('',*,*,#2071,.T.);
#2697=ORIENTED_EDGE('',*,*,#2072,.F.);
#2698=ORIENTED_EDGE('',*,*,#2073,.F.);
#2699=ORIENTED_EDGE('',*,*,#2074,.F.);
#2700=ORIENTED_EDGE('',*,*,#2075,.T.);
#2701=ORIENTED_EDGE('',*,*,#2055,.T.);
#2702=ORIENTED_EDGE('',*,*,#2058,.T.);
#2703=ORIENTED_EDGE('',*,*,#2066,.T.);
#2704=ORIENTED_EDGE('',*,*,#2076,.T.);
#2705=ORIENTED_EDGE('',*,*,#2077,.T.);
#2706=ORIENTED_EDGE('',*,*,#2078,.T.);
#2707=ORIENTED_EDGE('',*,*,#2076,.F.);
#2708=ORIENTED_EDGE('',*,*,#2065,.T.);
#2709=ORIENTED_EDGE('',*,*,#2079,.F.);
#2710=ORIENTED_EDGE('',*,*,#2080,.T.);
#2711=ORIENTED_EDGE('',*,*,#2081,.T.);
#2712=ORIENTED_EDGE('',*,*,#2082,.T.);
#2713=ORIENTED_EDGE('',*,*,#2072,.T.);
#2714=ORIENTED_EDGE('',*,*,#2083,.T.);
#2715=ORIENTED_EDGE('',*,*,#2083,.F.);
#2716=ORIENTED_EDGE('',*,*,#2071,.F.);
#2717=ORIENTED_EDGE('',*,*,#2084,.T.);
#2718=ORIENTED_EDGE('',*,*,#2085,.F.);
#2719=ORIENTED_EDGE('',*,*,#2086,.T.);
#2720=ORIENTED_EDGE('',*,*,#2079,.T.);
#2721=ORIENTED_EDGE('',*,*,#2064,.T.);
#2722=ORIENTED_EDGE('',*,*,#2087,.T.);
#2723=ORIENTED_EDGE('',*,*,#2087,.F.);
#2724=ORIENTED_EDGE('',*,*,#2063,.F.);
#2725=ORIENTED_EDGE('',*,*,#2061,.F.);
#2726=ORIENTED_EDGE('',*,*,#2088,.T.);
#2727=ORIENTED_EDGE('',*,*,#2089,.F.);
#2728=ORIENTED_EDGE('',*,*,#2074,.T.);
#2729=ORIENTED_EDGE('',*,*,#2090,.T.);
#2730=ORIENTED_EDGE('',*,*,#2091,.T.);
#2731=ORIENTED_EDGE('',*,*,#2092,.T.);
#2732=ORIENTED_EDGE('',*,*,#2092,.F.);
#2733=ORIENTED_EDGE('',*,*,#2093,.F.);
#2734=ORIENTED_EDGE('',*,*,#2094,.T.);
#2735=ORIENTED_EDGE('',*,*,#2059,.T.);
#2736=ORIENTED_EDGE('',*,*,#2075,.F.);
#2737=ORIENTED_EDGE('',*,*,#2095,.F.);
#2738=ORIENTED_EDGE('',*,*,#2096,.F.);
#2739=ORIENTED_EDGE('',*,*,#2068,.F.);
#2740=ORIENTED_EDGE('',*,*,#2097,.T.);
#2741=ORIENTED_EDGE('',*,*,#2078,.F.);
#2742=ORIENTED_EDGE('',*,*,#2098,.F.);
#2743=ORIENTED_EDGE('',*,*,#2097,.F.);
#2744=ORIENTED_EDGE('',*,*,#2067,.F.);
#2745=ORIENTED_EDGE('',*,*,#2099,.F.);
#2746=ORIENTED_EDGE('',*,*,#2084,.F.);
#2747=ORIENTED_EDGE('',*,*,#2070,.F.);
#2748=ORIENTED_EDGE('',*,*,#2100,.T.);
#2749=ORIENTED_EDGE('',*,*,#2101,.F.);
#2750=ORIENTED_EDGE('',*,*,#2100,.F.);
#2751=ORIENTED_EDGE('',*,*,#2069,.F.);
#2752=ORIENTED_EDGE('',*,*,#2096,.T.);
#2753=ORIENTED_EDGE('',*,*,#2088,.F.);
#2754=ORIENTED_EDGE('',*,*,#2102,.F.);
#2755=ORIENTED_EDGE('',*,*,#2103,.F.);
#2756=ORIENTED_EDGE('',*,*,#2104,.F.);
#2757=ORIENTED_EDGE('',*,*,#2105,.T.);
#2758=ORIENTED_EDGE('',*,*,#2077,.F.);
#2759=ORIENTED_EDGE('',*,*,#2080,.F.);
#2760=ORIENTED_EDGE('',*,*,#2086,.F.);
#2761=ORIENTED_EDGE('',*,*,#2089,.T.);
#2762=ORIENTED_EDGE('',*,*,#2105,.F.);
#2763=ORIENTED_EDGE('',*,*,#2106,.T.);
#2764=ORIENTED_EDGE('',*,*,#2107,.T.);
#2765=ORIENTED_EDGE('',*,*,#2093,.T.);
#2766=ORIENTED_EDGE('',*,*,#2091,.F.);
#2767=ORIENTED_EDGE('',*,*,#2108,.F.);
#2768=ORIENTED_EDGE('',*,*,#2081,.F.);
#2769=ORIENTED_EDGE('',*,*,#2085,.T.);
#2770=ORIENTED_EDGE('',*,*,#2099,.T.);
#2771=ORIENTED_EDGE('',*,*,#2101,.T.);
#2772=ORIENTED_EDGE('',*,*,#2095,.T.);
#2773=ORIENTED_EDGE('',*,*,#2098,.T.);
#2774=ORIENTED_EDGE('',*,*,#2082,.F.);
#2775=ORIENTED_EDGE('',*,*,#2108,.T.);
#2776=ORIENTED_EDGE('',*,*,#2090,.F.);
#2777=ORIENTED_EDGE('',*,*,#2073,.T.);
#2778=ORIENTED_EDGE('',*,*,#2109,.T.);
#2779=ORIENTED_EDGE('',*,*,#2110,.T.);
#2780=ORIENTED_EDGE('',*,*,#2111,.F.);
#2781=ORIENTED_EDGE('',*,*,#2112,.F.);
#2782=ORIENTED_EDGE('',*,*,#2113,.T.);
#2783=ORIENTED_EDGE('',*,*,#2112,.T.);
#2784=ORIENTED_EDGE('',*,*,#2114,.F.);
#2785=ORIENTED_EDGE('',*,*,#2115,.F.);
#2786=ORIENTED_EDGE('',*,*,#2116,.T.);
#2787=ORIENTED_EDGE('',*,*,#2115,.T.);
#2788=ORIENTED_EDGE('',*,*,#2117,.F.);
#2789=ORIENTED_EDGE('',*,*,#2118,.F.);
#2790=ORIENTED_EDGE('',*,*,#2119,.T.);
#2791=ORIENTED_EDGE('',*,*,#2118,.T.);
#2792=ORIENTED_EDGE('',*,*,#2120,.F.);
#2793=ORIENTED_EDGE('',*,*,#2110,.F.);
#2794=ORIENTED_EDGE('',*,*,#2121,.T.);
#2795=ORIENTED_EDGE('',*,*,#2122,.T.);
#2796=ORIENTED_EDGE('',*,*,#2123,.F.);
#2797=ORIENTED_EDGE('',*,*,#2124,.F.);
#2798=ORIENTED_EDGE('',*,*,#2125,.T.);
#2799=ORIENTED_EDGE('',*,*,#2124,.T.);
#2800=ORIENTED_EDGE('',*,*,#2126,.F.);
#2801=ORIENTED_EDGE('',*,*,#2127,.F.);
#2802=ORIENTED_EDGE('',*,*,#2128,.T.);
#2803=ORIENTED_EDGE('',*,*,#2127,.T.);
#2804=ORIENTED_EDGE('',*,*,#2129,.F.);
#2805=ORIENTED_EDGE('',*,*,#2130,.F.);
#2806=ORIENTED_EDGE('',*,*,#2131,.T.);
#2807=ORIENTED_EDGE('',*,*,#2130,.T.);
#2808=ORIENTED_EDGE('',*,*,#2132,.F.);
#2809=ORIENTED_EDGE('',*,*,#2122,.F.);
#2810=ORIENTED_EDGE('',*,*,#2094,.F.);
#2811=ORIENTED_EDGE('',*,*,#2107,.F.);
#2812=ORIENTED_EDGE('',*,*,#2133,.T.);
#2813=ORIENTED_EDGE('',*,*,#2134,.T.);
#2814=ORIENTED_EDGE('',*,*,#2135,.F.);
#2815=ORIENTED_EDGE('',*,*,#2136,.T.);
#2816=ORIENTED_EDGE('',*,*,#2103,.T.);
#2817=ORIENTED_EDGE('',*,*,#2137,.F.);
#2818=ORIENTED_EDGE('',*,*,#2138,.F.);
#2819=ORIENTED_EDGE('',*,*,#2139,.F.);
#2820=ORIENTED_EDGE('',*,*,#2138,.T.);
#2821=ORIENTED_EDGE('',*,*,#2140,.F.);
#2822=ORIENTED_EDGE('',*,*,#2141,.F.);
#2823=ORIENTED_EDGE('',*,*,#2142,.T.);
#2824=ORIENTED_EDGE('',*,*,#2141,.T.);
#2825=ORIENTED_EDGE('',*,*,#2143,.F.);
#2826=ORIENTED_EDGE('',*,*,#2134,.F.);
#2827=ORIENTED_EDGE('',*,*,#2060,.F.);
#2828=ORIENTED_EDGE('',*,*,#2135,.T.);
#2829=ORIENTED_EDGE('',*,*,#2143,.T.);
#2830=ORIENTED_EDGE('',*,*,#2140,.T.);
#2831=ORIENTED_EDGE('',*,*,#2137,.T.);
#2832=ORIENTED_EDGE('',*,*,#2102,.T.);
#2833=ORIENTED_EDGE('',*,*,#2132,.T.);
#2834=ORIENTED_EDGE('',*,*,#2129,.T.);
#2835=ORIENTED_EDGE('',*,*,#2126,.T.);
#2836=ORIENTED_EDGE('',*,*,#2123,.T.);
#2837=ORIENTED_EDGE('',*,*,#2120,.T.);
#2838=ORIENTED_EDGE('',*,*,#2117,.T.);
#2839=ORIENTED_EDGE('',*,*,#2114,.T.);
#2840=ORIENTED_EDGE('',*,*,#2111,.T.);
#2841=ORIENTED_EDGE('',*,*,#2142,.F.);
#2842=ORIENTED_EDGE('',*,*,#2133,.F.);
#2843=ORIENTED_EDGE('',*,*,#2106,.F.);
#2844=ORIENTED_EDGE('',*,*,#2104,.T.);
#2845=ORIENTED_EDGE('',*,*,#2136,.F.);
#2846=ORIENTED_EDGE('',*,*,#2139,.T.);
#2847=ORIENTED_EDGE('',*,*,#2131,.F.);
#2848=ORIENTED_EDGE('',*,*,#2121,.F.);
#2849=ORIENTED_EDGE('',*,*,#2125,.F.);
#2850=ORIENTED_EDGE('',*,*,#2128,.F.);
#2851=ORIENTED_EDGE('',*,*,#2119,.F.);
#2852=ORIENTED_EDGE('',*,*,#2109,.F.);
#2853=ORIENTED_EDGE('',*,*,#2113,.F.);
#2854=ORIENTED_EDGE('',*,*,#2116,.F.);
#2855=ORIENTED_EDGE('',*,*,#2144,.F.);
#2856=ORIENTED_EDGE('',*,*,#2145,.T.);
#2857=ORIENTED_EDGE('',*,*,#2146,.F.);
#2858=ORIENTED_EDGE('',*,*,#2145,.F.);
#2859=ORIENTED_EDGE('',*,*,#2144,.T.);
#2860=ORIENTED_EDGE('',*,*,#2147,.F.);
#2861=ORIENTED_EDGE('',*,*,#2148,.T.);
#2862=ORIENTED_EDGE('',*,*,#2149,.F.);
#2863=ORIENTED_EDGE('',*,*,#2148,.F.);
#2864=ORIENTED_EDGE('',*,*,#2147,.T.);
#2865=ORIENTED_EDGE('',*,*,#2150,.T.);
#2866=ORIENTED_EDGE('',*,*,#2151,.T.);
#2867=ORIENTED_EDGE('',*,*,#2152,.F.);
#2868=ORIENTED_EDGE('',*,*,#2153,.T.);
#2869=ORIENTED_EDGE('',*,*,#2153,.F.);
#2870=ORIENTED_EDGE('',*,*,#2154,.F.);
#2871=ORIENTED_EDGE('',*,*,#2155,.F.);
#2872=ORIENTED_EDGE('',*,*,#2156,.F.);
#2873=ORIENTED_EDGE('',*,*,#2157,.F.);
#2874=ORIENTED_EDGE('',*,*,#2158,.F.);
#2875=ORIENTED_EDGE('',*,*,#2159,.F.);
#2876=ORIENTED_EDGE('',*,*,#2160,.F.);
#2877=ORIENTED_EDGE('',*,*,#2161,.F.);
#2878=ORIENTED_EDGE('',*,*,#2162,.F.);
#2879=ORIENTED_EDGE('',*,*,#2163,.F.);
#2880=ORIENTED_EDGE('',*,*,#2164,.F.);
#2881=ORIENTED_EDGE('',*,*,#2165,.F.);
#2882=ORIENTED_EDGE('',*,*,#2166,.F.);
#2883=ORIENTED_EDGE('',*,*,#2167,.F.);
#2884=ORIENTED_EDGE('',*,*,#2168,.F.);
#2885=ORIENTED_EDGE('',*,*,#2169,.F.);
#2886=ORIENTED_EDGE('',*,*,#2170,.F.);
#2887=ORIENTED_EDGE('',*,*,#2170,.T.);
#2888=ORIENTED_EDGE('',*,*,#2171,.F.);
#2889=ORIENTED_EDGE('',*,*,#2172,.T.);
#2890=ORIENTED_EDGE('',*,*,#2173,.F.);
#2891=ORIENTED_EDGE('',*,*,#2151,.F.);
#2892=ORIENTED_EDGE('',*,*,#2174,.F.);
#2893=ORIENTED_EDGE('',*,*,#2175,.T.);
#2894=ORIENTED_EDGE('',*,*,#2176,.T.);
#2895=ORIENTED_EDGE('',*,*,#2177,.T.);
#2896=ORIENTED_EDGE('',*,*,#2178,.F.);
#2897=ORIENTED_EDGE('',*,*,#2179,.F.);
#2898=ORIENTED_EDGE('',*,*,#2180,.F.);
#2899=ORIENTED_EDGE('',*,*,#2181,.F.);
#2900=ORIENTED_EDGE('',*,*,#2182,.F.);
#2901=ORIENTED_EDGE('',*,*,#2167,.T.);
#2902=ORIENTED_EDGE('',*,*,#2173,.T.);
#2903=ORIENTED_EDGE('',*,*,#2183,.T.);
#2904=ORIENTED_EDGE('',*,*,#2184,.F.);
#2905=ORIENTED_EDGE('',*,*,#2146,.T.);
#2906=ORIENTED_EDGE('',*,*,#2149,.T.);
#2907=ORIENTED_EDGE('',*,*,#2185,.F.);
#2908=ORIENTED_EDGE('',*,*,#2186,.F.);
#2909=ORIENTED_EDGE('',*,*,#2177,.F.);
#2910=ORIENTED_EDGE('',*,*,#2187,.F.);
#2911=ORIENTED_EDGE('',*,*,#2186,.T.);
#2912=ORIENTED_EDGE('',*,*,#2188,.T.);
#2913=ORIENTED_EDGE('',*,*,#2189,.F.);
#2914=ORIENTED_EDGE('',*,*,#2178,.T.);
#2915=ORIENTED_EDGE('',*,*,#2190,.F.);
#2916=ORIENTED_EDGE('',*,*,#2191,.F.);
#2917=ORIENTED_EDGE('',*,*,#2183,.F.);
#2918=ORIENTED_EDGE('',*,*,#2172,.F.);
#2919=ORIENTED_EDGE('',*,*,#2191,.T.);
#2920=ORIENTED_EDGE('',*,*,#2192,.T.);
#2921=ORIENTED_EDGE('',*,*,#2193,.F.);
#2922=ORIENTED_EDGE('',*,*,#2152,.T.);
#2923=ORIENTED_EDGE('',*,*,#2184,.T.);
#2924=ORIENTED_EDGE('',*,*,#2175,.F.);
#2925=ORIENTED_EDGE('',*,*,#2194,.F.);
#2926=ORIENTED_EDGE('',*,*,#2195,.F.);
#2927=ORIENTED_EDGE('',*,*,#2196,.F.);
#2928=ORIENTED_EDGE('',*,*,#2194,.T.);
#2929=ORIENTED_EDGE('',*,*,#2174,.T.);
#2930=ORIENTED_EDGE('',*,*,#2150,.F.);
#2931=ORIENTED_EDGE('',*,*,#2197,.T.);
#2932=ORIENTED_EDGE('',*,*,#2198,.T.);
#2933=ORIENTED_EDGE('',*,*,#2199,.T.);
#2934=ORIENTED_EDGE('',*,*,#2200,.F.);
#2935=ORIENTED_EDGE('',*,*,#2181,.T.);
#2936=ORIENTED_EDGE('',*,*,#2201,.T.);
#2937=ORIENTED_EDGE('',*,*,#2168,.T.);
#2938=ORIENTED_EDGE('',*,*,#2182,.T.);
#2939=ORIENTED_EDGE('',*,*,#2200,.T.);
#2940=ORIENTED_EDGE('',*,*,#2202,.T.);
#2941=ORIENTED_EDGE('',*,*,#2203,.T.);
#2942=ORIENTED_EDGE('',*,*,#2204,.F.);
#2943=ORIENTED_EDGE('',*,*,#2179,.T.);
#2944=ORIENTED_EDGE('',*,*,#2189,.T.);
#2945=ORIENTED_EDGE('',*,*,#2205,.T.);
#2946=ORIENTED_EDGE('',*,*,#2201,.F.);
#2947=ORIENTED_EDGE('',*,*,#2180,.T.);
#2948=ORIENTED_EDGE('',*,*,#2204,.T.);
#2949=ORIENTED_EDGE('',*,*,#2193,.T.);
#2950=ORIENTED_EDGE('',*,*,#2206,.F.);
#2951=ORIENTED_EDGE('',*,*,#2207,.T.);
#2952=ORIENTED_EDGE('',*,*,#2208,.T.);
#2953=ORIENTED_EDGE('',*,*,#2154,.T.);
#2954=ORIENTED_EDGE('',*,*,#2169,.T.);
#2955=ORIENTED_EDGE('',*,*,#2202,.F.);
#2956=ORIENTED_EDGE('',*,*,#2199,.F.);
#2957=ORIENTED_EDGE('',*,*,#2205,.F.);
#2958=ORIENTED_EDGE('',*,*,#2203,.F.);
#2959=ORIENTED_EDGE('',*,*,#2188,.F.);
#2960=ORIENTED_EDGE('',*,*,#2185,.T.);
#2961=ORIENTED_EDGE('',*,*,#2209,.T.);
#2962=ORIENTED_EDGE('',*,*,#2195,.T.);
#2963=ORIENTED_EDGE('',*,*,#2198,.F.);
#2964=ORIENTED_EDGE('',*,*,#2210,.F.);
#2965=ORIENTED_EDGE('',*,*,#2211,.F.);
#2966=ORIENTED_EDGE('',*,*,#2206,.T.);
#2967=ORIENTED_EDGE('',*,*,#2192,.F.);
#2968=ORIENTED_EDGE('',*,*,#2190,.T.);
#2969=ORIENTED_EDGE('',*,*,#2171,.T.);
#2970=ORIENTED_EDGE('',*,*,#2187,.T.);
#2971=ORIENTED_EDGE('',*,*,#2176,.F.);
#2972=ORIENTED_EDGE('',*,*,#2196,.T.);
#2973=ORIENTED_EDGE('',*,*,#2209,.F.);
#2974=ORIENTED_EDGE('',*,*,#2212,.F.);
#2975=ORIENTED_EDGE('',*,*,#2213,.T.);
#2976=ORIENTED_EDGE('',*,*,#2160,.T.);
#2977=ORIENTED_EDGE('',*,*,#2214,.F.);
#2978=ORIENTED_EDGE('',*,*,#2215,.F.);
#2979=ORIENTED_EDGE('',*,*,#2216,.T.);
#2980=ORIENTED_EDGE('',*,*,#2161,.T.);
#2981=ORIENTED_EDGE('',*,*,#2213,.F.);
#2982=ORIENTED_EDGE('',*,*,#2217,.F.);
#2983=ORIENTED_EDGE('',*,*,#2218,.T.);
#2984=ORIENTED_EDGE('',*,*,#2162,.T.);
#2985=ORIENTED_EDGE('',*,*,#2216,.F.);
#2986=ORIENTED_EDGE('',*,*,#2219,.F.);
#2987=ORIENTED_EDGE('',*,*,#2214,.T.);
#2988=ORIENTED_EDGE('',*,*,#2159,.T.);
#2989=ORIENTED_EDGE('',*,*,#2218,.F.);
#2990=ORIENTED_EDGE('',*,*,#2220,.F.);
#2991=ORIENTED_EDGE('',*,*,#2221,.T.);
#2992=ORIENTED_EDGE('',*,*,#2164,.T.);
#2993=ORIENTED_EDGE('',*,*,#2222,.F.);
#2994=ORIENTED_EDGE('',*,*,#2223,.F.);
#2995=ORIENTED_EDGE('',*,*,#2224,.T.);
#2996=ORIENTED_EDGE('',*,*,#2165,.T.);
#2997=ORIENTED_EDGE('',*,*,#2221,.F.);
#2998=ORIENTED_EDGE('',*,*,#2225,.F.);
#2999=ORIENTED_EDGE('',*,*,#2226,.T.);
#3000=ORIENTED_EDGE('',*,*,#2166,.T.);
#3001=ORIENTED_EDGE('',*,*,#2224,.F.);
#3002=ORIENTED_EDGE('',*,*,#2227,.F.);
#3003=ORIENTED_EDGE('',*,*,#2222,.T.);
#3004=ORIENTED_EDGE('',*,*,#2163,.T.);
#3005=ORIENTED_EDGE('',*,*,#2226,.F.);
#3006=ORIENTED_EDGE('',*,*,#2197,.F.);
#3007=ORIENTED_EDGE('',*,*,#2158,.T.);
#3008=ORIENTED_EDGE('',*,*,#2228,.F.);
#3009=ORIENTED_EDGE('',*,*,#2229,.F.);
#3010=ORIENTED_EDGE('',*,*,#2210,.T.);
#3011=ORIENTED_EDGE('',*,*,#2230,.F.);
#3012=ORIENTED_EDGE('',*,*,#2231,.T.);
#3013=ORIENTED_EDGE('',*,*,#2155,.T.);
#3014=ORIENTED_EDGE('',*,*,#2208,.F.);
#3015=ORIENTED_EDGE('',*,*,#2232,.T.);
#3016=ORIENTED_EDGE('',*,*,#2233,.T.);
#3017=ORIENTED_EDGE('',*,*,#2156,.T.);
#3018=ORIENTED_EDGE('',*,*,#2231,.F.);
#3019=ORIENTED_EDGE('',*,*,#2234,.F.);
#3020=ORIENTED_EDGE('',*,*,#2228,.T.);
#3021=ORIENTED_EDGE('',*,*,#2157,.T.);
#3022=ORIENTED_EDGE('',*,*,#2233,.F.);
#3023=ORIENTED_EDGE('',*,*,#2234,.T.);
#3024=ORIENTED_EDGE('',*,*,#2232,.F.);
#3025=ORIENTED_EDGE('',*,*,#2230,.T.);
#3026=ORIENTED_EDGE('',*,*,#2207,.F.);
#3027=ORIENTED_EDGE('',*,*,#2211,.T.);
#3028=ORIENTED_EDGE('',*,*,#2229,.T.);
#3029=ORIENTED_EDGE('',*,*,#2227,.T.);
#3030=ORIENTED_EDGE('',*,*,#2225,.T.);
#3031=ORIENTED_EDGE('',*,*,#2223,.T.);
#3032=ORIENTED_EDGE('',*,*,#2220,.T.);
#3033=ORIENTED_EDGE('',*,*,#2219,.T.);
#3034=ORIENTED_EDGE('',*,*,#2217,.T.);
#3035=ORIENTED_EDGE('',*,*,#2215,.T.);
#3036=ORIENTED_EDGE('',*,*,#2212,.T.);
#3037=ORIENTED_EDGE('',*,*,#2235,.F.);
#3038=ORIENTED_EDGE('',*,*,#2236,.T.);
#3039=ORIENTED_EDGE('',*,*,#2237,.F.);
#3040=ORIENTED_EDGE('',*,*,#2236,.F.);
#3041=ORIENTED_EDGE('',*,*,#2238,.F.);
#3042=ORIENTED_EDGE('',*,*,#2239,.T.);
#3043=ORIENTED_EDGE('',*,*,#2240,.F.);
#3044=ORIENTED_EDGE('',*,*,#2241,.F.);
#3045=ORIENTED_EDGE('',*,*,#2242,.F.);
#3046=ORIENTED_EDGE('',*,*,#2241,.T.);
#3047=ORIENTED_EDGE('',*,*,#2243,.F.);
#3048=ORIENTED_EDGE('',*,*,#2244,.F.);
#3049=ORIENTED_EDGE('',*,*,#2245,.F.);
#3050=ORIENTED_EDGE('',*,*,#2244,.T.);
#3051=ORIENTED_EDGE('',*,*,#2246,.F.);
#3052=ORIENTED_EDGE('',*,*,#2247,.F.);
#3053=ORIENTED_EDGE('',*,*,#2248,.F.);
#3054=ORIENTED_EDGE('',*,*,#2247,.T.);
#3055=ORIENTED_EDGE('',*,*,#2249,.F.);
#3056=ORIENTED_EDGE('',*,*,#2250,.F.);
#3057=ORIENTED_EDGE('',*,*,#2251,.F.);
#3058=ORIENTED_EDGE('',*,*,#2250,.T.);
#3059=ORIENTED_EDGE('',*,*,#2252,.F.);
#3060=ORIENTED_EDGE('',*,*,#2253,.F.);
#3061=ORIENTED_EDGE('',*,*,#2254,.F.);
#3062=ORIENTED_EDGE('',*,*,#2253,.T.);
#3063=ORIENTED_EDGE('',*,*,#2255,.F.);
#3064=ORIENTED_EDGE('',*,*,#2239,.F.);
#3065=ORIENTED_EDGE('',*,*,#2254,.T.);
#3066=ORIENTED_EDGE('',*,*,#2238,.T.);
#3067=ORIENTED_EDGE('',*,*,#2242,.T.);
#3068=ORIENTED_EDGE('',*,*,#2245,.T.);
#3069=ORIENTED_EDGE('',*,*,#2248,.T.);
#3070=ORIENTED_EDGE('',*,*,#2251,.T.);
#3071=ORIENTED_EDGE('',*,*,#2235,.T.);
#3072=ORIENTED_EDGE('',*,*,#2255,.T.);
#3073=ORIENTED_EDGE('',*,*,#2252,.T.);
#3074=ORIENTED_EDGE('',*,*,#2249,.T.);
#3075=ORIENTED_EDGE('',*,*,#2246,.T.);
#3076=ORIENTED_EDGE('',*,*,#2243,.T.);
#3077=ORIENTED_EDGE('',*,*,#2240,.T.);
#3078=ORIENTED_EDGE('',*,*,#2237,.T.);
#3079=ORIENTED_EDGE('',*,*,#2256,.F.);
#3080=ORIENTED_EDGE('',*,*,#2257,.F.);
#3081=ORIENTED_EDGE('',*,*,#2258,.F.);
#3082=ORIENTED_EDGE('',*,*,#2259,.T.);
#3083=ORIENTED_EDGE('',*,*,#2260,.F.);
#3084=ORIENTED_EDGE('',*,*,#2261,.F.);
#3085=ORIENTED_EDGE('',*,*,#2256,.T.);
#3086=ORIENTED_EDGE('',*,*,#2262,.T.);
#3087=ORIENTED_EDGE('',*,*,#2263,.F.);
#3088=ORIENTED_EDGE('',*,*,#2264,.F.);
#3089=ORIENTED_EDGE('',*,*,#2260,.T.);
#3090=ORIENTED_EDGE('',*,*,#2265,.T.);
#3091=ORIENTED_EDGE('',*,*,#2266,.F.);
#3092=ORIENTED_EDGE('',*,*,#2267,.F.);
#3093=ORIENTED_EDGE('',*,*,#2263,.T.);
#3094=ORIENTED_EDGE('',*,*,#2268,.T.);
#3095=ORIENTED_EDGE('',*,*,#2269,.F.);
#3096=ORIENTED_EDGE('',*,*,#2270,.F.);
#3097=ORIENTED_EDGE('',*,*,#2266,.T.);
#3098=ORIENTED_EDGE('',*,*,#2271,.T.);
#3099=ORIENTED_EDGE('',*,*,#2272,.F.);
#3100=ORIENTED_EDGE('',*,*,#2273,.F.);
#3101=ORIENTED_EDGE('',*,*,#2269,.T.);
#3102=ORIENTED_EDGE('',*,*,#2274,.T.);
#3103=ORIENTED_EDGE('',*,*,#2275,.F.);
#3104=ORIENTED_EDGE('',*,*,#2276,.F.);
#3105=ORIENTED_EDGE('',*,*,#2272,.T.);
#3106=ORIENTED_EDGE('',*,*,#2277,.T.);
#3107=ORIENTED_EDGE('',*,*,#2278,.F.);
#3108=ORIENTED_EDGE('',*,*,#2279,.F.);
#3109=ORIENTED_EDGE('',*,*,#2275,.T.);
#3110=ORIENTED_EDGE('',*,*,#2280,.T.);
#3111=ORIENTED_EDGE('',*,*,#2281,.F.);
#3112=ORIENTED_EDGE('',*,*,#2282,.F.);
#3113=ORIENTED_EDGE('',*,*,#2278,.T.);
#3114=ORIENTED_EDGE('',*,*,#2283,.T.);
#3115=ORIENTED_EDGE('',*,*,#2284,.F.);
#3116=ORIENTED_EDGE('',*,*,#2285,.F.);
#3117=ORIENTED_EDGE('',*,*,#2281,.T.);
#3118=ORIENTED_EDGE('',*,*,#2286,.T.);
#3119=ORIENTED_EDGE('',*,*,#2287,.F.);
#3120=ORIENTED_EDGE('',*,*,#2288,.F.);
#3121=ORIENTED_EDGE('',*,*,#2284,.T.);
#3122=ORIENTED_EDGE('',*,*,#2289,.T.);
#3123=ORIENTED_EDGE('',*,*,#2290,.T.);
#3124=ORIENTED_EDGE('',*,*,#2291,.F.);
#3125=ORIENTED_EDGE('',*,*,#2292,.F.);
#3126=ORIENTED_EDGE('',*,*,#2287,.T.);
#3127=ORIENTED_EDGE('',*,*,#2293,.T.);
#3128=ORIENTED_EDGE('',*,*,#2294,.F.);
#3129=ORIENTED_EDGE('',*,*,#2295,.F.);
#3130=ORIENTED_EDGE('',*,*,#2296,.F.);
#3131=ORIENTED_EDGE('',*,*,#2291,.T.);
#3132=ORIENTED_EDGE('',*,*,#2297,.T.);
#3133=ORIENTED_EDGE('',*,*,#2298,.F.);
#3134=ORIENTED_EDGE('',*,*,#2299,.F.);
#3135=ORIENTED_EDGE('',*,*,#2294,.T.);
#3136=ORIENTED_EDGE('',*,*,#2300,.T.);
#3137=ORIENTED_EDGE('',*,*,#2301,.F.);
#3138=ORIENTED_EDGE('',*,*,#2302,.F.);
#3139=ORIENTED_EDGE('',*,*,#2298,.T.);
#3140=ORIENTED_EDGE('',*,*,#2303,.T.);
#3141=ORIENTED_EDGE('',*,*,#2304,.F.);
#3142=ORIENTED_EDGE('',*,*,#2305,.F.);
#3143=ORIENTED_EDGE('',*,*,#2301,.T.);
#3144=ORIENTED_EDGE('',*,*,#2306,.T.);
#3145=ORIENTED_EDGE('',*,*,#2307,.F.);
#3146=ORIENTED_EDGE('',*,*,#2308,.F.);
#3147=ORIENTED_EDGE('',*,*,#2304,.T.);
#3148=ORIENTED_EDGE('',*,*,#2309,.T.);
#3149=ORIENTED_EDGE('',*,*,#2310,.F.);
#3150=ORIENTED_EDGE('',*,*,#2311,.F.);
#3151=ORIENTED_EDGE('',*,*,#2307,.T.);
#3152=ORIENTED_EDGE('',*,*,#2312,.T.);
#3153=ORIENTED_EDGE('',*,*,#2313,.F.);
#3154=ORIENTED_EDGE('',*,*,#2314,.F.);
#3155=ORIENTED_EDGE('',*,*,#2310,.T.);
#3156=ORIENTED_EDGE('',*,*,#2315,.T.);
#3157=ORIENTED_EDGE('',*,*,#2316,.F.);
#3158=ORIENTED_EDGE('',*,*,#2317,.F.);
#3159=ORIENTED_EDGE('',*,*,#2313,.T.);
#3160=ORIENTED_EDGE('',*,*,#2318,.T.);
#3161=ORIENTED_EDGE('',*,*,#2319,.F.);
#3162=ORIENTED_EDGE('',*,*,#2320,.F.);
#3163=ORIENTED_EDGE('',*,*,#2316,.T.);
#3164=ORIENTED_EDGE('',*,*,#2321,.T.);
#3165=ORIENTED_EDGE('',*,*,#2322,.F.);
#3166=ORIENTED_EDGE('',*,*,#2323,.F.);
#3167=ORIENTED_EDGE('',*,*,#2319,.T.);
#3168=ORIENTED_EDGE('',*,*,#2324,.T.);
#3169=ORIENTED_EDGE('',*,*,#2325,.T.);
#3170=ORIENTED_EDGE('',*,*,#2326,.F.);
#3171=ORIENTED_EDGE('',*,*,#2327,.T.);
#3172=ORIENTED_EDGE('',*,*,#2328,.T.);
#3173=ORIENTED_EDGE('',*,*,#2329,.T.);
#3174=ORIENTED_EDGE('',*,*,#2330,.T.);
#3175=ORIENTED_EDGE('',*,*,#2331,.T.);
#3176=ORIENTED_EDGE('',*,*,#2332,.T.);
#3177=ORIENTED_EDGE('',*,*,#2333,.T.);
#3178=ORIENTED_EDGE('',*,*,#2334,.T.);
#3179=ORIENTED_EDGE('',*,*,#2335,.T.);
#3180=ORIENTED_EDGE('',*,*,#2336,.T.);
#3181=ORIENTED_EDGE('',*,*,#2337,.T.);
#3182=ORIENTED_EDGE('',*,*,#2338,.T.);
#3183=ORIENTED_EDGE('',*,*,#2339,.T.);
#3184=ORIENTED_EDGE('',*,*,#2340,.T.);
#3185=ORIENTED_EDGE('',*,*,#2341,.T.);
#3186=ORIENTED_EDGE('',*,*,#2342,.T.);
#3187=ORIENTED_EDGE('',*,*,#2343,.T.);
#3188=ORIENTED_EDGE('',*,*,#2344,.T.);
#3189=ORIENTED_EDGE('',*,*,#2345,.T.);
#3190=ORIENTED_EDGE('',*,*,#2346,.T.);
#3191=ORIENTED_EDGE('',*,*,#2347,.T.);
#3192=ORIENTED_EDGE('',*,*,#2348,.T.);
#3193=ORIENTED_EDGE('',*,*,#2349,.T.);
#3194=ORIENTED_EDGE('',*,*,#2350,.T.);
#3195=ORIENTED_EDGE('',*,*,#2351,.F.);
#3196=ORIENTED_EDGE('',*,*,#2352,.T.);
#3197=ORIENTED_EDGE('',*,*,#2353,.T.);
#3198=ORIENTED_EDGE('',*,*,#2354,.T.);
#3199=ORIENTED_EDGE('',*,*,#2355,.T.);
#3200=ORIENTED_EDGE('',*,*,#2356,.T.);
#3201=ORIENTED_EDGE('',*,*,#2357,.T.);
#3202=ORIENTED_EDGE('',*,*,#2358,.T.);
#3203=ORIENTED_EDGE('',*,*,#2359,.T.);
#3204=ORIENTED_EDGE('',*,*,#2360,.T.);
#3205=ORIENTED_EDGE('',*,*,#2361,.T.);
#3206=ORIENTED_EDGE('',*,*,#2362,.T.);
#3207=ORIENTED_EDGE('',*,*,#2363,.T.);
#3208=ORIENTED_EDGE('',*,*,#2364,.T.);
#3209=ORIENTED_EDGE('',*,*,#2365,.T.);
#3210=ORIENTED_EDGE('',*,*,#2366,.T.);
#3211=ORIENTED_EDGE('',*,*,#2367,.T.);
#3212=ORIENTED_EDGE('',*,*,#2368,.T.);
#3213=ORIENTED_EDGE('',*,*,#2369,.T.);
#3214=ORIENTED_EDGE('',*,*,#2370,.T.);
#3215=ORIENTED_EDGE('',*,*,#2371,.T.);
#3216=ORIENTED_EDGE('',*,*,#2372,.T.);
#3217=ORIENTED_EDGE('',*,*,#2373,.T.);
#3218=ORIENTED_EDGE('',*,*,#2374,.T.);
#3219=ORIENTED_EDGE('',*,*,#2322,.T.);
#3220=ORIENTED_EDGE('',*,*,#2375,.T.);
#3221=ORIENTED_EDGE('',*,*,#2376,.F.);
#3222=ORIENTED_EDGE('',*,*,#2377,.F.);
#3223=ORIENTED_EDGE('',*,*,#2378,.F.);
#3224=ORIENTED_EDGE('',*,*,#2350,.F.);
#3225=ORIENTED_EDGE('',*,*,#2349,.F.);
#3226=ORIENTED_EDGE('',*,*,#2348,.F.);
#3227=ORIENTED_EDGE('',*,*,#2347,.F.);
#3228=ORIENTED_EDGE('',*,*,#2346,.F.);
#3229=ORIENTED_EDGE('',*,*,#2345,.F.);
#3230=ORIENTED_EDGE('',*,*,#2344,.F.);
#3231=ORIENTED_EDGE('',*,*,#2343,.F.);
#3232=ORIENTED_EDGE('',*,*,#2342,.F.);
#3233=ORIENTED_EDGE('',*,*,#2341,.F.);
#3234=ORIENTED_EDGE('',*,*,#2340,.F.);
#3235=ORIENTED_EDGE('',*,*,#2339,.F.);
#3236=ORIENTED_EDGE('',*,*,#2338,.F.);
#3237=ORIENTED_EDGE('',*,*,#2337,.F.);
#3238=ORIENTED_EDGE('',*,*,#2336,.F.);
#3239=ORIENTED_EDGE('',*,*,#2335,.F.);
#3240=ORIENTED_EDGE('',*,*,#2334,.F.);
#3241=ORIENTED_EDGE('',*,*,#2333,.F.);
#3242=ORIENTED_EDGE('',*,*,#2332,.F.);
#3243=ORIENTED_EDGE('',*,*,#2331,.F.);
#3244=ORIENTED_EDGE('',*,*,#2330,.F.);
#3245=ORIENTED_EDGE('',*,*,#2329,.F.);
#3246=ORIENTED_EDGE('',*,*,#2328,.F.);
#3247=ORIENTED_EDGE('',*,*,#2327,.F.);
#3248=ORIENTED_EDGE('',*,*,#2379,.F.);
#3249=ORIENTED_EDGE('',*,*,#2380,.T.);
#3250=ORIENTED_EDGE('',*,*,#2257,.T.);
#3251=ORIENTED_EDGE('',*,*,#2261,.T.);
#3252=ORIENTED_EDGE('',*,*,#2264,.T.);
#3253=ORIENTED_EDGE('',*,*,#2267,.T.);
#3254=ORIENTED_EDGE('',*,*,#2270,.T.);
#3255=ORIENTED_EDGE('',*,*,#2273,.T.);
#3256=ORIENTED_EDGE('',*,*,#2276,.T.);
#3257=ORIENTED_EDGE('',*,*,#2279,.T.);
#3258=ORIENTED_EDGE('',*,*,#2282,.T.);
#3259=ORIENTED_EDGE('',*,*,#2285,.T.);
#3260=ORIENTED_EDGE('',*,*,#2288,.T.);
#3261=ORIENTED_EDGE('',*,*,#2292,.T.);
#3262=ORIENTED_EDGE('',*,*,#2296,.T.);
#3263=ORIENTED_EDGE('',*,*,#2295,.T.);
#3264=ORIENTED_EDGE('',*,*,#2299,.T.);
#3265=ORIENTED_EDGE('',*,*,#2302,.T.);
#3266=ORIENTED_EDGE('',*,*,#2305,.T.);
#3267=ORIENTED_EDGE('',*,*,#2308,.T.);
#3268=ORIENTED_EDGE('',*,*,#2311,.T.);
#3269=ORIENTED_EDGE('',*,*,#2314,.T.);
#3270=ORIENTED_EDGE('',*,*,#2317,.T.);
#3271=ORIENTED_EDGE('',*,*,#2320,.T.);
#3272=ORIENTED_EDGE('',*,*,#2323,.T.);
#3273=ORIENTED_EDGE('',*,*,#2377,.T.);
#3274=ORIENTED_EDGE('',*,*,#2381,.F.);
#3275=ORIENTED_EDGE('',*,*,#2382,.F.);
#3276=ORIENTED_EDGE('',*,*,#2375,.F.);
#3277=ORIENTED_EDGE('',*,*,#2324,.F.);
#3278=ORIENTED_EDGE('',*,*,#2321,.F.);
#3279=ORIENTED_EDGE('',*,*,#2318,.F.);
#3280=ORIENTED_EDGE('',*,*,#2315,.F.);
#3281=ORIENTED_EDGE('',*,*,#2312,.F.);
#3282=ORIENTED_EDGE('',*,*,#2309,.F.);
#3283=ORIENTED_EDGE('',*,*,#2306,.F.);
#3284=ORIENTED_EDGE('',*,*,#2303,.F.);
#3285=ORIENTED_EDGE('',*,*,#2300,.F.);
#3286=ORIENTED_EDGE('',*,*,#2297,.F.);
#3287=ORIENTED_EDGE('',*,*,#2293,.F.);
#3288=ORIENTED_EDGE('',*,*,#2290,.F.);
#3289=ORIENTED_EDGE('',*,*,#2289,.F.);
#3290=ORIENTED_EDGE('',*,*,#2286,.F.);
#3291=ORIENTED_EDGE('',*,*,#2283,.F.);
#3292=ORIENTED_EDGE('',*,*,#2280,.F.);
#3293=ORIENTED_EDGE('',*,*,#2277,.F.);
#3294=ORIENTED_EDGE('',*,*,#2274,.F.);
#3295=ORIENTED_EDGE('',*,*,#2271,.F.);
#3296=ORIENTED_EDGE('',*,*,#2268,.F.);
#3297=ORIENTED_EDGE('',*,*,#2265,.F.);
#3298=ORIENTED_EDGE('',*,*,#2262,.F.);
#3299=ORIENTED_EDGE('',*,*,#2259,.F.);
#3300=ORIENTED_EDGE('',*,*,#2383,.F.);
#3301=ORIENTED_EDGE('',*,*,#2325,.F.);
#3302=ORIENTED_EDGE('',*,*,#2374,.F.);
#3303=ORIENTED_EDGE('',*,*,#2373,.F.);
#3304=ORIENTED_EDGE('',*,*,#2372,.F.);
#3305=ORIENTED_EDGE('',*,*,#2371,.F.);
#3306=ORIENTED_EDGE('',*,*,#2370,.F.);
#3307=ORIENTED_EDGE('',*,*,#2369,.F.);
#3308=ORIENTED_EDGE('',*,*,#2368,.F.);
#3309=ORIENTED_EDGE('',*,*,#2367,.F.);
#3310=ORIENTED_EDGE('',*,*,#2366,.F.);
#3311=ORIENTED_EDGE('',*,*,#2365,.F.);
#3312=ORIENTED_EDGE('',*,*,#2364,.F.);
#3313=ORIENTED_EDGE('',*,*,#2363,.F.);
#3314=ORIENTED_EDGE('',*,*,#2362,.F.);
#3315=ORIENTED_EDGE('',*,*,#2361,.F.);
#3316=ORIENTED_EDGE('',*,*,#2360,.F.);
#3317=ORIENTED_EDGE('',*,*,#2359,.F.);
#3318=ORIENTED_EDGE('',*,*,#2358,.F.);
#3319=ORIENTED_EDGE('',*,*,#2357,.F.);
#3320=ORIENTED_EDGE('',*,*,#2356,.F.);
#3321=ORIENTED_EDGE('',*,*,#2355,.F.);
#3322=ORIENTED_EDGE('',*,*,#2354,.F.);
#3323=ORIENTED_EDGE('',*,*,#2353,.F.);
#3324=ORIENTED_EDGE('',*,*,#2352,.F.);
#3325=ORIENTED_EDGE('',*,*,#2381,.T.);
#3326=ORIENTED_EDGE('',*,*,#2351,.T.);
#3327=ORIENTED_EDGE('',*,*,#2378,.T.);
#3328=ORIENTED_EDGE('',*,*,#2376,.T.);
#3329=ORIENTED_EDGE('',*,*,#2382,.T.);
#3330=ORIENTED_EDGE('',*,*,#2384,.F.);
#3331=ORIENTED_EDGE('',*,*,#2326,.T.);
#3332=ORIENTED_EDGE('',*,*,#2383,.T.);
#3333=ORIENTED_EDGE('',*,*,#2258,.T.);
#3334=ORIENTED_EDGE('',*,*,#2380,.F.);
#3335=ORIENTED_EDGE('',*,*,#2379,.T.);
#3336=ORIENTED_EDGE('',*,*,#2385,.F.);
#3337=ORIENTED_EDGE('',*,*,#2386,.T.);
#3338=ORIENTED_EDGE('',*,*,#2384,.T.);
#3339=ORIENTED_EDGE('',*,*,#2386,.F.);
#3340=ORIENTED_EDGE('',*,*,#2385,.T.);
#3341=ORIENTED_EDGE('',*,*,#2387,.T.);
#3342=ORIENTED_EDGE('',*,*,#2388,.F.);
#3343=ORIENTED_EDGE('',*,*,#2387,.F.);
#3344=ORIENTED_EDGE('',*,*,#2388,.T.);
#3345=ORIENTED_EDGE('',*,*,#2389,.F.);
#3346=ORIENTED_EDGE('',*,*,#2390,.T.);
#3347=ORIENTED_EDGE('',*,*,#2391,.F.);
#3348=ORIENTED_EDGE('',*,*,#2390,.F.);
#3349=ORIENTED_EDGE('',*,*,#2392,.F.);
#3350=ORIENTED_EDGE('',*,*,#2393,.T.);
#3351=ORIENTED_EDGE('',*,*,#2394,.F.);
#3352=ORIENTED_EDGE('',*,*,#2395,.F.);
#3353=ORIENTED_EDGE('',*,*,#2396,.F.);
#3354=ORIENTED_EDGE('',*,*,#2395,.T.);
#3355=ORIENTED_EDGE('',*,*,#2397,.F.);
#3356=ORIENTED_EDGE('',*,*,#2398,.F.);
#3357=ORIENTED_EDGE('',*,*,#2399,.F.);
#3358=ORIENTED_EDGE('',*,*,#2398,.T.);
#3359=ORIENTED_EDGE('',*,*,#2400,.F.);
#3360=ORIENTED_EDGE('',*,*,#2401,.F.);
#3361=ORIENTED_EDGE('',*,*,#2402,.F.);
#3362=ORIENTED_EDGE('',*,*,#2401,.T.);
#3363=ORIENTED_EDGE('',*,*,#2403,.F.);
#3364=ORIENTED_EDGE('',*,*,#2404,.F.);
#3365=ORIENTED_EDGE('',*,*,#2405,.F.);
#3366=ORIENTED_EDGE('',*,*,#2404,.T.);
#3367=ORIENTED_EDGE('',*,*,#2406,.F.);
#3368=ORIENTED_EDGE('',*,*,#2407,.F.);
#3369=ORIENTED_EDGE('',*,*,#2408,.F.);
#3370=ORIENTED_EDGE('',*,*,#2407,.T.);
#3371=ORIENTED_EDGE('',*,*,#2409,.F.);
#3372=ORIENTED_EDGE('',*,*,#2393,.F.);
#3373=ORIENTED_EDGE('',*,*,#2408,.T.);
#3374=ORIENTED_EDGE('',*,*,#2392,.T.);
#3375=ORIENTED_EDGE('',*,*,#2396,.T.);
#3376=ORIENTED_EDGE('',*,*,#2399,.T.);
#3377=ORIENTED_EDGE('',*,*,#2402,.T.);
#3378=ORIENTED_EDGE('',*,*,#2405,.T.);
#3379=ORIENTED_EDGE('',*,*,#2389,.T.);
#3380=ORIENTED_EDGE('',*,*,#2409,.T.);
#3381=ORIENTED_EDGE('',*,*,#2406,.T.);
#3382=ORIENTED_EDGE('',*,*,#2403,.T.);
#3383=ORIENTED_EDGE('',*,*,#2400,.T.);
#3384=ORIENTED_EDGE('',*,*,#2397,.T.);
#3385=ORIENTED_EDGE('',*,*,#2394,.T.);
#3386=ORIENTED_EDGE('',*,*,#2391,.T.);
#3387=ORIENTED_EDGE('',*,*,#2410,.T.);
#3388=ORIENTED_EDGE('',*,*,#2411,.T.);
#3389=ORIENTED_EDGE('',*,*,#2412,.T.);
#3390=ORIENTED_EDGE('',*,*,#2413,.T.);
#3391=ORIENTED_EDGE('',*,*,#2414,.T.);
#3392=ORIENTED_EDGE('',*,*,#2415,.T.);
#3393=ORIENTED_EDGE('',*,*,#2412,.F.);
#3394=ORIENTED_EDGE('',*,*,#2416,.T.);
#3395=ORIENTED_EDGE('',*,*,#2413,.F.);
#3396=ORIENTED_EDGE('',*,*,#2417,.T.);
#3397=ORIENTED_EDGE('',*,*,#2418,.F.);
#3398=ORIENTED_EDGE('',*,*,#2419,.F.);
#3399=ORIENTED_EDGE('',*,*,#2415,.F.);
#3400=ORIENTED_EDGE('',*,*,#2420,.T.);
#3401=ORIENTED_EDGE('',*,*,#2421,.F.);
#3402=ORIENTED_EDGE('',*,*,#2417,.F.);
#3403=ORIENTED_EDGE('',*,*,#2414,.F.);
#3404=ORIENTED_EDGE('',*,*,#2422,.T.);
#3405=ORIENTED_EDGE('',*,*,#2423,.F.);
#3406=ORIENTED_EDGE('',*,*,#2424,.F.);
#3407=ORIENTED_EDGE('',*,*,#2425,.T.);
#3408=ORIENTED_EDGE('',*,*,#2426,.F.);
#3409=ORIENTED_EDGE('',*,*,#2427,.F.);
#3410=ORIENTED_EDGE('',*,*,#2420,.F.);
#3411=ORIENTED_EDGE('',*,*,#2428,.T.);
#3412=ORIENTED_EDGE('',*,*,#2418,.T.);
#3413=ORIENTED_EDGE('',*,*,#2429,.T.);
#3414=ORIENTED_EDGE('',*,*,#2430,.T.);
#3415=ORIENTED_EDGE('',*,*,#2427,.T.);
#3416=ORIENTED_EDGE('',*,*,#2431,.T.);
#3417=ORIENTED_EDGE('',*,*,#2429,.F.);
#3418=ORIENTED_EDGE('',*,*,#2421,.T.);
#3419=ORIENTED_EDGE('',*,*,#2430,.F.);
#3420=ORIENTED_EDGE('',*,*,#2431,.F.);
#3421=ORIENTED_EDGE('',*,*,#2426,.T.);
#3422=ORIENTED_EDGE('',*,*,#2432,.T.);
#3423=ORIENTED_EDGE('',*,*,#2433,.T.);
#3424=ORIENTED_EDGE('',*,*,#2434,.T.);
#3425=ORIENTED_EDGE('',*,*,#2435,.T.);
#3426=ORIENTED_EDGE('',*,*,#2436,.T.);
#3427=ORIENTED_EDGE('',*,*,#2437,.T.);
#3428=ORIENTED_EDGE('',*,*,#2438,.T.);
#3429=ORIENTED_EDGE('',*,*,#2439,.T.);
#3430=ORIENTED_EDGE('',*,*,#2440,.T.);
#3431=ORIENTED_EDGE('',*,*,#2441,.T.);
#3432=ORIENTED_EDGE('',*,*,#2442,.T.);
#3433=ORIENTED_EDGE('',*,*,#2439,.F.);
#3434=ORIENTED_EDGE('',*,*,#2442,.F.);
#3435=ORIENTED_EDGE('',*,*,#2441,.F.);
#3436=ORIENTED_EDGE('',*,*,#2443,.T.);
#3437=ORIENTED_EDGE('',*,*,#2444,.T.);
#3438=ORIENTED_EDGE('',*,*,#2445,.T.);
#3439=ORIENTED_EDGE('',*,*,#2438,.F.);
#3440=ORIENTED_EDGE('',*,*,#2445,.F.);
#3441=ORIENTED_EDGE('',*,*,#2444,.F.);
#3442=ORIENTED_EDGE('',*,*,#2446,.F.);
#3443=ORIENTED_EDGE('',*,*,#2447,.F.);
#3444=ORIENTED_EDGE('',*,*,#2448,.T.);
#3445=ORIENTED_EDGE('',*,*,#2449,.F.);
#3446=ORIENTED_EDGE('',*,*,#2448,.F.);
#3447=ORIENTED_EDGE('',*,*,#2447,.T.);
#3448=ORIENTED_EDGE('',*,*,#2450,.F.);
#3449=ORIENTED_EDGE('',*,*,#2451,.F.);
#3450=ORIENTED_EDGE('',*,*,#2452,.T.);
#3451=ORIENTED_EDGE('',*,*,#2453,.F.);
#3452=ORIENTED_EDGE('',*,*,#2452,.F.);
#3453=ORIENTED_EDGE('',*,*,#2451,.T.);
#3454=ORIENTED_EDGE('',*,*,#2450,.T.);
#3455=ORIENTED_EDGE('',*,*,#2454,.T.);
#3456=ORIENTED_EDGE('',*,*,#2455,.F.);
#3457=ORIENTED_EDGE('',*,*,#2454,.F.);
#3458=ORIENTED_EDGE('',*,*,#2446,.T.);
#3459=ORIENTED_EDGE('',*,*,#2456,.T.);
#3460=ORIENTED_EDGE('',*,*,#2457,.F.);
#3461=ORIENTED_EDGE('',*,*,#2456,.F.);
#3462=ORIENTED_EDGE('',*,*,#2458,.T.);
#3463=ORIENTED_EDGE('',*,*,#2423,.T.);
#3464=ORIENTED_EDGE('',*,*,#2459,.T.);
#3465=ORIENTED_EDGE('',*,*,#2460,.F.);
#3466=ORIENTED_EDGE('',*,*,#2461,.F.);
#3467=ORIENTED_EDGE('',*,*,#2462,.T.);
#3468=ORIENTED_EDGE('',*,*,#2463,.T.);
#3469=ORIENTED_EDGE('',*,*,#2464,.F.);
#3470=ORIENTED_EDGE('',*,*,#2465,.F.);
#3471=ORIENTED_EDGE('',*,*,#2466,.T.);
#3472=ORIENTED_EDGE('',*,*,#2467,.T.);
#3473=ORIENTED_EDGE('',*,*,#2462,.F.);
#3474=ORIENTED_EDGE('',*,*,#2468,.T.);
#3475=ORIENTED_EDGE('',*,*,#2469,.T.);
#3476=ORIENTED_EDGE('',*,*,#2470,.T.);
#3477=ORIENTED_EDGE('',*,*,#2466,.F.);
#3478=ORIENTED_EDGE('',*,*,#2471,.F.);
#3479=ORIENTED_EDGE('',*,*,#2460,.T.);
#3480=ORIENTED_EDGE('',*,*,#2472,.T.);
#3481=ORIENTED_EDGE('',*,*,#2469,.F.);
#3482=ORIENTED_EDGE('',*,*,#2411,.F.);
#3483=ORIENTED_EDGE('',*,*,#2473,.F.);
#3484=ORIENTED_EDGE('',*,*,#2463,.F.);
#3485=ORIENTED_EDGE('',*,*,#2467,.F.);
#3486=ORIENTED_EDGE('',*,*,#2470,.F.);
#3487=ORIENTED_EDGE('',*,*,#2472,.F.);
#3488=ORIENTED_EDGE('',*,*,#2459,.F.);
#3489=ORIENTED_EDGE('',*,*,#2422,.F.);
#3490=ORIENTED_EDGE('',*,*,#2416,.F.);
#3491=ORIENTED_EDGE('',*,*,#2449,.T.);
#3492=ORIENTED_EDGE('',*,*,#2453,.T.);
#3493=ORIENTED_EDGE('',*,*,#2474,.F.);
#3494=ORIENTED_EDGE('',*,*,#2458,.F.);
#3495=ORIENTED_EDGE('',*,*,#2471,.T.);
#3496=ORIENTED_EDGE('',*,*,#2468,.F.);
#3497=ORIENTED_EDGE('',*,*,#2465,.T.);
#3498=ORIENTED_EDGE('',*,*,#2461,.T.);
#3499=ORIENTED_EDGE('',*,*,#2475,.F.);
#3500=ORIENTED_EDGE('',*,*,#2476,.F.);
#3501=ORIENTED_EDGE('',*,*,#2477,.F.);
#3502=ORIENTED_EDGE('',*,*,#2457,.T.);
#3503=ORIENTED_EDGE('',*,*,#2455,.T.);
#3504=ORIENTED_EDGE('',*,*,#2474,.T.);
#3505=ORIENTED_EDGE('',*,*,#2478,.F.);
#3506=ORIENTED_EDGE('',*,*,#2479,.F.);
#3507=ORIENTED_EDGE('',*,*,#2424,.T.);
#3508=ORIENTED_EDGE('',*,*,#2477,.T.);
#3509=ORIENTED_EDGE('',*,*,#2480,.F.);
#3510=ORIENTED_EDGE('',*,*,#2481,.F.);
#3511=ORIENTED_EDGE('',*,*,#2478,.T.);
#3512=ORIENTED_EDGE('',*,*,#2476,.T.);
#3513=ORIENTED_EDGE('',*,*,#2482,.F.);
#3514=ORIENTED_EDGE('',*,*,#2483,.F.);
#3515=ORIENTED_EDGE('',*,*,#2480,.T.);
#3516=ORIENTED_EDGE('',*,*,#2479,.T.);
#3517=ORIENTED_EDGE('',*,*,#2481,.T.);
#3518=ORIENTED_EDGE('',*,*,#2483,.T.);
#3519=ORIENTED_EDGE('',*,*,#2484,.T.);
#3520=ORIENTED_EDGE('',*,*,#2485,.F.);
#3521=ORIENTED_EDGE('',*,*,#2486,.F.);
#3522=ORIENTED_EDGE('',*,*,#2487,.T.);
#3523=ORIENTED_EDGE('',*,*,#2488,.F.);
#3524=ORIENTED_EDGE('',*,*,#2489,.T.);
#3525=ORIENTED_EDGE('',*,*,#2490,.F.);
#3526=ORIENTED_EDGE('',*,*,#2491,.F.);
#3527=ORIENTED_EDGE('',*,*,#2490,.T.);
#3528=ORIENTED_EDGE('',*,*,#2492,.T.);
#3529=ORIENTED_EDGE('',*,*,#2443,.F.);
#3530=ORIENTED_EDGE('',*,*,#2492,.F.);
#3531=ORIENTED_EDGE('',*,*,#2491,.T.);
#3532=ORIENTED_EDGE('',*,*,#2493,.T.);
#3533=ORIENTED_EDGE('',*,*,#2440,.F.);
#3534=ORIENTED_EDGE('',*,*,#2493,.F.);
#3535=ORIENTED_EDGE('',*,*,#2489,.F.);
#3536=ORIENTED_EDGE('',*,*,#2494,.T.);
#3537=ORIENTED_EDGE('',*,*,#2432,.F.);
#3538=ORIENTED_EDGE('',*,*,#2425,.F.);
#3539=ORIENTED_EDGE('',*,*,#2410,.F.);
#3540=ORIENTED_EDGE('',*,*,#2419,.T.);
#3541=ORIENTED_EDGE('',*,*,#2428,.F.);
#3542=ORIENTED_EDGE('',*,*,#2437,.F.);
#3543=ORIENTED_EDGE('',*,*,#2495,.F.);
#3544=ORIENTED_EDGE('',*,*,#2484,.F.);
#3545=ORIENTED_EDGE('',*,*,#2482,.T.);
#3546=ORIENTED_EDGE('',*,*,#2475,.T.);
#3547=ORIENTED_EDGE('',*,*,#2464,.T.);
#3548=ORIENTED_EDGE('',*,*,#2473,.T.);
#3549=ORIENTED_EDGE('',*,*,#2485,.T.);
#3550=ORIENTED_EDGE('',*,*,#2495,.T.);
#3551=ORIENTED_EDGE('',*,*,#2436,.F.);
#3552=ORIENTED_EDGE('',*,*,#2496,.F.);
#3553=ORIENTED_EDGE('',*,*,#2486,.T.);
#3554=ORIENTED_EDGE('',*,*,#2496,.T.);
#3555=ORIENTED_EDGE('',*,*,#2435,.F.);
#3556=ORIENTED_EDGE('',*,*,#2497,.F.);
#3557=ORIENTED_EDGE('',*,*,#2487,.F.);
#3558=ORIENTED_EDGE('',*,*,#2497,.T.);
#3559=ORIENTED_EDGE('',*,*,#2434,.F.);
#3560=ORIENTED_EDGE('',*,*,#2498,.F.);
#3561=ORIENTED_EDGE('',*,*,#2488,.T.);
#3562=ORIENTED_EDGE('',*,*,#2498,.T.);
#3563=ORIENTED_EDGE('',*,*,#2433,.F.);
#3564=ORIENTED_EDGE('',*,*,#2494,.F.);
#3565=ORIENTED_EDGE('',*,*,#2499,.F.);
#3566=ORIENTED_EDGE('',*,*,#2500,.T.);
#3567=ORIENTED_EDGE('',*,*,#2501,.F.);
#3568=ORIENTED_EDGE('',*,*,#2502,.F.);
#3569=ORIENTED_EDGE('',*,*,#2503,.F.);
#3570=ORIENTED_EDGE('',*,*,#2504,.F.);
#3571=ORIENTED_EDGE('',*,*,#2505,.T.);
#3572=ORIENTED_EDGE('',*,*,#2506,.F.);
#3573=ORIENTED_EDGE('',*,*,#2507,.F.);
#3574=ORIENTED_EDGE('',*,*,#2508,.T.);
#3575=ORIENTED_EDGE('',*,*,#2509,.F.);
#3576=ORIENTED_EDGE('',*,*,#2510,.F.);
#3577=ORIENTED_EDGE('',*,*,#2502,.T.);
#3578=ORIENTED_EDGE('',*,*,#2511,.F.);
#3579=ORIENTED_EDGE('',*,*,#2512,.F.);
#3580=ORIENTED_EDGE('',*,*,#2513,.F.);
#3581=ORIENTED_EDGE('',*,*,#2514,.F.);
#3582=ORIENTED_EDGE('',*,*,#2515,.F.);
#3583=ORIENTED_EDGE('',*,*,#2516,.F.);
#3584=ORIENTED_EDGE('',*,*,#2517,.F.);
#3585=ORIENTED_EDGE('',*,*,#2518,.T.);
#3586=ORIENTED_EDGE('',*,*,#2519,.F.);
#3587=ORIENTED_EDGE('',*,*,#2500,.F.);
#3588=ORIENTED_EDGE('',*,*,#2520,.F.);
#3589=ORIENTED_EDGE('',*,*,#2521,.T.);
#3590=ORIENTED_EDGE('',*,*,#2522,.F.);
#3591=ORIENTED_EDGE('',*,*,#2523,.F.);
#3592=ORIENTED_EDGE('',*,*,#2524,.F.);
#3593=ORIENTED_EDGE('',*,*,#2505,.F.);
#3594=ORIENTED_EDGE('',*,*,#2525,.F.);
#3595=ORIENTED_EDGE('',*,*,#2521,.F.);
#3596=ORIENTED_EDGE('',*,*,#2503,.T.);
#3597=ORIENTED_EDGE('',*,*,#2526,.T.);
#3598=ORIENTED_EDGE('',*,*,#2527,.F.);
#3599=ORIENTED_EDGE('',*,*,#2528,.T.);
#3600=ORIENTED_EDGE('',*,*,#2529,.T.);
#3601=ORIENTED_EDGE('',*,*,#2530,.F.);
#3602=ORIENTED_EDGE('',*,*,#2531,.F.);
#3603=ORIENTED_EDGE('',*,*,#2532,.F.);
#3604=ORIENTED_EDGE('',*,*,#2533,.F.);
#3605=ORIENTED_EDGE('',*,*,#2517,.T.);
#3606=ORIENTED_EDGE('',*,*,#2499,.T.);
#3607=ORIENTED_EDGE('',*,*,#2510,.T.);
#3608=ORIENTED_EDGE('',*,*,#2506,.T.);
#3609=ORIENTED_EDGE('',*,*,#2524,.T.);
#3610=ORIENTED_EDGE('',*,*,#2520,.T.);
#3611=ORIENTED_EDGE('',*,*,#2534,.T.);
#3612=ORIENTED_EDGE('',*,*,#2535,.F.);
#3613=ORIENTED_EDGE('',*,*,#2536,.F.);
#3614=ORIENTED_EDGE('',*,*,#2526,.F.);
#3615=ORIENTED_EDGE('',*,*,#2537,.F.);
#3616=ORIENTED_EDGE('',*,*,#2538,.F.);
#3617=ORIENTED_EDGE('',*,*,#2529,.F.);
#3618=ORIENTED_EDGE('',*,*,#2509,.T.);
#3619=ORIENTED_EDGE('',*,*,#2539,.T.);
#3620=ORIENTED_EDGE('',*,*,#2540,.T.);
#3621=ORIENTED_EDGE('',*,*,#2537,.T.);
#3622=ORIENTED_EDGE('',*,*,#2508,.F.);
#3623=ORIENTED_EDGE('',*,*,#2541,.F.);
#3624=ORIENTED_EDGE('',*,*,#2542,.F.);
#3625=ORIENTED_EDGE('',*,*,#2539,.F.);
#3626=ORIENTED_EDGE('',*,*,#2507,.T.);
#3627=ORIENTED_EDGE('',*,*,#2543,.T.);
#3628=ORIENTED_EDGE('',*,*,#2544,.F.);
#3629=ORIENTED_EDGE('',*,*,#2545,.F.);
#3630=ORIENTED_EDGE('',*,*,#2513,.T.);
#3631=ORIENTED_EDGE('',*,*,#2546,.T.);
#3632=ORIENTED_EDGE('',*,*,#2547,.F.);
#3633=ORIENTED_EDGE('',*,*,#2543,.F.);
#3634=ORIENTED_EDGE('',*,*,#2512,.T.);
#3635=ORIENTED_EDGE('',*,*,#2546,.F.);
#3636=ORIENTED_EDGE('',*,*,#2511,.T.);
#3637=ORIENTED_EDGE('',*,*,#2501,.T.);
#3638=ORIENTED_EDGE('',*,*,#2519,.T.);
#3639=ORIENTED_EDGE('',*,*,#2548,.F.);
#3640=ORIENTED_EDGE('',*,*,#2549,.F.);
#3641=ORIENTED_EDGE('',*,*,#2550,.F.);
#3642=ORIENTED_EDGE('',*,*,#2551,.F.);
#3643=ORIENTED_EDGE('',*,*,#2528,.F.);
#3644=ORIENTED_EDGE('',*,*,#2552,.F.);
#3645=ORIENTED_EDGE('',*,*,#2553,.F.);
#3646=ORIENTED_EDGE('',*,*,#2554,.T.);
#3647=ORIENTED_EDGE('',*,*,#2522,.T.);
#3648=ORIENTED_EDGE('',*,*,#2525,.T.);
#3649=ORIENTED_EDGE('',*,*,#2504,.T.);
#3650=ORIENTED_EDGE('',*,*,#2555,.F.);
#3651=ORIENTED_EDGE('',*,*,#2556,.T.);
#3652=ORIENTED_EDGE('',*,*,#2515,.T.);
#3653=ORIENTED_EDGE('',*,*,#2556,.F.);
#3654=ORIENTED_EDGE('',*,*,#2557,.F.);
#3655=ORIENTED_EDGE('',*,*,#2558,.T.);
#3656=ORIENTED_EDGE('',*,*,#2516,.T.);
#3657=ORIENTED_EDGE('',*,*,#2558,.F.);
#3658=ORIENTED_EDGE('',*,*,#2545,.T.);
#3659=ORIENTED_EDGE('',*,*,#2559,.F.);
#3660=ORIENTED_EDGE('',*,*,#2541,.T.);
#3661=ORIENTED_EDGE('',*,*,#2514,.T.);
#3662=ORIENTED_EDGE('',*,*,#2531,.T.);
#3663=ORIENTED_EDGE('',*,*,#2560,.T.);
#3664=ORIENTED_EDGE('',*,*,#2550,.T.);
#3665=ORIENTED_EDGE('',*,*,#2561,.F.);
#3666=ORIENTED_EDGE('',*,*,#2542,.T.);
#3667=ORIENTED_EDGE('',*,*,#2559,.T.);
#3668=ORIENTED_EDGE('',*,*,#2544,.T.);
#3669=ORIENTED_EDGE('',*,*,#2547,.T.);
#3670=ORIENTED_EDGE('',*,*,#2551,.T.);
#3671=ORIENTED_EDGE('',*,*,#2560,.F.);
#3672=ORIENTED_EDGE('',*,*,#2530,.T.);
#3673=ORIENTED_EDGE('',*,*,#2538,.T.);
#3674=ORIENTED_EDGE('',*,*,#2540,.F.);
#3675=ORIENTED_EDGE('',*,*,#2555,.T.);
#3676=ORIENTED_EDGE('',*,*,#2557,.T.);
#3677=ORIENTED_EDGE('',*,*,#2532,.T.);
#3678=ORIENTED_EDGE('',*,*,#2561,.T.);
#3679=ORIENTED_EDGE('',*,*,#2549,.T.);
#3680=ORIENTED_EDGE('',*,*,#2562,.F.);
#3681=ORIENTED_EDGE('',*,*,#2533,.T.);
#3682=ORIENTED_EDGE('',*,*,#2562,.T.);
#3683=ORIENTED_EDGE('',*,*,#2548,.T.);
#3684=ORIENTED_EDGE('',*,*,#2518,.F.);
#3685=ORIENTED_EDGE('',*,*,#2534,.F.);
#3686=ORIENTED_EDGE('',*,*,#2523,.T.);
#3687=ORIENTED_EDGE('',*,*,#2554,.F.);
#3688=ORIENTED_EDGE('',*,*,#2563,.F.);
#3689=ORIENTED_EDGE('',*,*,#2535,.T.);
#3690=ORIENTED_EDGE('',*,*,#2563,.T.);
#3691=ORIENTED_EDGE('',*,*,#2553,.T.);
#3692=ORIENTED_EDGE('',*,*,#2564,.F.);
#3693=ORIENTED_EDGE('',*,*,#2536,.T.);
#3694=ORIENTED_EDGE('',*,*,#2564,.T.);
#3695=ORIENTED_EDGE('',*,*,#2552,.T.);
#3696=ORIENTED_EDGE('',*,*,#2527,.T.);
#3697=ORIENTED_EDGE('',*,*,#2565,.T.);
#3698=ORIENTED_EDGE('',*,*,#2566,.T.);
#3699=ORIENTED_EDGE('',*,*,#2567,.T.);
#3700=ORIENTED_EDGE('',*,*,#2568,.T.);
#3701=ORIENTED_EDGE('',*,*,#2569,.T.);
#3702=ORIENTED_EDGE('',*,*,#2570,.T.);
#3703=ORIENTED_EDGE('',*,*,#2571,.T.);
#3704=ORIENTED_EDGE('',*,*,#2572,.T.);
#3705=ORIENTED_EDGE('',*,*,#2573,.T.);
#3706=ORIENTED_EDGE('',*,*,#2574,.T.);
#3707=ORIENTED_EDGE('',*,*,#2575,.T.);
#3708=ORIENTED_EDGE('',*,*,#2576,.T.);
#3709=ORIENTED_EDGE('',*,*,#2570,.F.);
#3710=ORIENTED_EDGE('',*,*,#2577,.T.);
#3711=ORIENTED_EDGE('',*,*,#2578,.T.);
#3712=ORIENTED_EDGE('',*,*,#2579,.T.);
#3713=ORIENTED_EDGE('',*,*,#2575,.F.);
#3714=ORIENTED_EDGE('',*,*,#2580,.T.);
#3715=ORIENTED_EDGE('',*,*,#2581,.T.);
#3716=ORIENTED_EDGE('',*,*,#2582,.T.);
#3717=ORIENTED_EDGE('',*,*,#2578,.F.);
#3718=ORIENTED_EDGE('',*,*,#2583,.T.);
#3719=ORIENTED_EDGE('',*,*,#2584,.T.);
#3720=ORIENTED_EDGE('',*,*,#2585,.T.);
#3721=ORIENTED_EDGE('',*,*,#2581,.F.);
#3722=ORIENTED_EDGE('',*,*,#2586,.T.);
#3723=ORIENTED_EDGE('',*,*,#2584,.F.);
#3724=ORIENTED_EDGE('',*,*,#2587,.T.);
#3725=ORIENTED_EDGE('',*,*,#2567,.F.);
#3726=ORIENTED_EDGE('',*,*,#2588,.T.);
#3727=ORIENTED_EDGE('',*,*,#2589,.T.);
#3728=ORIENTED_EDGE('',*,*,#2572,.F.);
#3729=ORIENTED_EDGE('',*,*,#2590,.T.);
#3730=ORIENTED_EDGE('',*,*,#2565,.F.);
#3731=ORIENTED_EDGE('',*,*,#2588,.F.);
#3732=ORIENTED_EDGE('',*,*,#2591,.F.);
#3733=ORIENTED_EDGE('',*,*,#2592,.F.);
#3734=ORIENTED_EDGE('',*,*,#2593,.F.);
#3735=ORIENTED_EDGE('',*,*,#2594,.F.);
#3736=ORIENTED_EDGE('',*,*,#2566,.F.);
#3737=ORIENTED_EDGE('',*,*,#2595,.T.);
#3738=ORIENTED_EDGE('',*,*,#2596,.T.);
#3739=ORIENTED_EDGE('',*,*,#2591,.T.);
#3740=ORIENTED_EDGE('',*,*,#2590,.F.);
#3741=ORIENTED_EDGE('',*,*,#2597,.F.);
#3742=ORIENTED_EDGE('',*,*,#2598,.F.);
#3743=ORIENTED_EDGE('',*,*,#2595,.F.);
#3744=ORIENTED_EDGE('',*,*,#2571,.F.);
#3745=ORIENTED_EDGE('',*,*,#2599,.T.);
#3746=ORIENTED_EDGE('',*,*,#2600,.T.);
#3747=ORIENTED_EDGE('',*,*,#2597,.T.);
#3748=ORIENTED_EDGE('',*,*,#2568,.F.);
#3749=ORIENTED_EDGE('',*,*,#2587,.F.);
#3750=ORIENTED_EDGE('',*,*,#2586,.F.);
#3751=ORIENTED_EDGE('',*,*,#2583,.F.);
#3752=ORIENTED_EDGE('',*,*,#2580,.F.);
#3753=ORIENTED_EDGE('',*,*,#2577,.F.);
#3754=ORIENTED_EDGE('',*,*,#2574,.F.);
#3755=ORIENTED_EDGE('',*,*,#2601,.T.);
#3756=ORIENTED_EDGE('',*,*,#2602,.T.);
#3757=ORIENTED_EDGE('',*,*,#2603,.F.);
#3758=ORIENTED_EDGE('',*,*,#2604,.T.);
#3759=ORIENTED_EDGE('',*,*,#2605,.T.);
#3760=ORIENTED_EDGE('',*,*,#2606,.T.);
#3761=ORIENTED_EDGE('',*,*,#2607,.T.);
#3762=ORIENTED_EDGE('',*,*,#2605,.F.);
#3763=ORIENTED_EDGE('',*,*,#2608,.T.);
#3764=ORIENTED_EDGE('',*,*,#2609,.T.);
#3765=ORIENTED_EDGE('',*,*,#2579,.F.);
#3766=ORIENTED_EDGE('',*,*,#2610,.T.);
#3767=ORIENTED_EDGE('',*,*,#2607,.F.);
#3768=ORIENTED_EDGE('',*,*,#2611,.T.);
#3769=ORIENTED_EDGE('',*,*,#2609,.F.);
#3770=ORIENTED_EDGE('',*,*,#2612,.T.);
#3771=ORIENTED_EDGE('',*,*,#2613,.F.);
#3772=ORIENTED_EDGE('',*,*,#2614,.T.);
#3773=ORIENTED_EDGE('',*,*,#2608,.F.);
#3774=ORIENTED_EDGE('',*,*,#2615,.T.);
#3775=ORIENTED_EDGE('',*,*,#2616,.F.);
#3776=ORIENTED_EDGE('',*,*,#2617,.T.);
#3777=ORIENTED_EDGE('',*,*,#2604,.F.);
#3778=ORIENTED_EDGE('',*,*,#2618,.F.);
#3779=ORIENTED_EDGE('',*,*,#2619,.F.);
#3780=ORIENTED_EDGE('',*,*,#2615,.F.);
#3781=ORIENTED_EDGE('',*,*,#2600,.F.);
#3782=ORIENTED_EDGE('',*,*,#2613,.T.);
#3783=ORIENTED_EDGE('',*,*,#2620,.T.);
#3784=ORIENTED_EDGE('',*,*,#2576,.F.);
#3785=ORIENTED_EDGE('',*,*,#2611,.F.);
#3786=ORIENTED_EDGE('',*,*,#2606,.F.);
#3787=ORIENTED_EDGE('',*,*,#2614,.F.);
#3788=ORIENTED_EDGE('',*,*,#2599,.F.);
#3789=ORIENTED_EDGE('',*,*,#2585,.F.);
#3790=ORIENTED_EDGE('',*,*,#2594,.T.);
#3791=ORIENTED_EDGE('',*,*,#2621,.T.);
#3792=ORIENTED_EDGE('',*,*,#2622,.T.);
#3793=ORIENTED_EDGE('',*,*,#2593,.T.);
#3794=ORIENTED_EDGE('',*,*,#2623,.T.);
#3795=ORIENTED_EDGE('',*,*,#2619,.T.);
#3796=ORIENTED_EDGE('',*,*,#2621,.F.);
#3797=ORIENTED_EDGE('',*,*,#2623,.F.);
#3798=ORIENTED_EDGE('',*,*,#2624,.T.);
#3799=ORIENTED_EDGE('',*,*,#2616,.T.);
#3800=ORIENTED_EDGE('',*,*,#2624,.F.);
#3801=ORIENTED_EDGE('',*,*,#2592,.T.);
#3802=ORIENTED_EDGE('',*,*,#2625,.F.);
#3803=ORIENTED_EDGE('',*,*,#2626,.T.);
#3804=ORIENTED_EDGE('',*,*,#2596,.F.);
#3805=ORIENTED_EDGE('',*,*,#2627,.T.);
#3806=ORIENTED_EDGE('',*,*,#2625,.T.);
#3807=ORIENTED_EDGE('',*,*,#2620,.F.);
#3808=ORIENTED_EDGE('',*,*,#2628,.T.);
#3809=ORIENTED_EDGE('',*,*,#2627,.F.);
#3810=ORIENTED_EDGE('',*,*,#2598,.T.);
#3811=ORIENTED_EDGE('',*,*,#2626,.F.);
#3812=ORIENTED_EDGE('',*,*,#2628,.F.);
#3813=ORIENTED_EDGE('',*,*,#2612,.F.);
#3814=ORIENTED_EDGE('',*,*,#2617,.F.);
#3815=ORIENTED_EDGE('',*,*,#2569,.F.);
#3816=ORIENTED_EDGE('',*,*,#2603,.T.);
#3817=ORIENTED_EDGE('',*,*,#2629,.F.);
#3818=ORIENTED_EDGE('',*,*,#2630,.F.);
#3819=ORIENTED_EDGE('',*,*,#2631,.F.);
#3820=ORIENTED_EDGE('',*,*,#2589,.F.);
#3821=ORIENTED_EDGE('',*,*,#2631,.T.);
#3822=ORIENTED_EDGE('',*,*,#2632,.F.);
#3823=ORIENTED_EDGE('',*,*,#2633,.F.);
#3824=ORIENTED_EDGE('',*,*,#2630,.T.);
#3825=ORIENTED_EDGE('',*,*,#2634,.F.);
#3826=ORIENTED_EDGE('',*,*,#2635,.F.);
#3827=ORIENTED_EDGE('',*,*,#2632,.T.);
#3828=ORIENTED_EDGE('',*,*,#2629,.T.);
#3829=ORIENTED_EDGE('',*,*,#2602,.F.);
#3830=ORIENTED_EDGE('',*,*,#2636,.F.);
#3831=ORIENTED_EDGE('',*,*,#2634,.T.);
#3832=ORIENTED_EDGE('',*,*,#2573,.F.);
#3833=ORIENTED_EDGE('',*,*,#2633,.T.);
#3834=ORIENTED_EDGE('',*,*,#2635,.T.);
#3835=ORIENTED_EDGE('',*,*,#2636,.T.);
#3836=ORIENTED_EDGE('',*,*,#2601,.F.);
#3837=ORIENTED_EDGE('',*,*,#2582,.F.);
#3838=ORIENTED_EDGE('',*,*,#2622,.F.);
#3839=ORIENTED_EDGE('',*,*,#2618,.T.);
#3840=ORIENTED_EDGE('',*,*,#2610,.F.);
#3841=CYLINDRICAL_SURFACE('',#4268,1.75974879114541);
#3842=CYLINDRICAL_SURFACE('',#4271,1.69478250292167);
#3843=CYLINDRICAL_SURFACE('',#4274,2.25974879114541);
#3844=CYLINDRICAL_SURFACE('',#4278,2.69478250292167);
#3845=CYLINDRICAL_SURFACE('',#4295,1.5);
#3846=CYLINDRICAL_SURFACE('',#4306,2.5);
#3847=CYLINDRICAL_SURFACE('',#4309,2.5);
#3848=CYLINDRICAL_SURFACE('',#4312,2.75);
#3849=CYLINDRICAL_SURFACE('',#4315,2.75);
#3850=CYLINDRICAL_SURFACE('',#4318,2.00000000000029);
#3851=CYLINDRICAL_SURFACE('',#4321,2.00000000000029);
#3852=CYLINDRICAL_SURFACE('',#4323,3.70283120062258);
#3853=CYLINDRICAL_SURFACE('',#4329,2.29663666580012);
#3854=CYLINDRICAL_SURFACE('',#4333,2.29663666580012);
#3855=CYLINDRICAL_SURFACE('',#4337,2.29663666580012);
#3856=CYLINDRICAL_SURFACE('',#4341,2.29663666580012);
#3857=CYLINDRICAL_SURFACE('',#4345,2.50000000000001);
#3858=CYLINDRICAL_SURFACE('',#4349,2.5);
#3859=CYLINDRICAL_SURFACE('',#4365,1.5);
#3860=CYLINDRICAL_SURFACE('',#4375,2.5);
#3861=CYLINDRICAL_SURFACE('',#4386,2.5);
#3862=CYLINDRICAL_SURFACE('',#4389,2.75);
#3863=CYLINDRICAL_SURFACE('',#4392,2.75);
#3864=CYLINDRICAL_SURFACE('',#4395,2.00000000000029);
#3865=CYLINDRICAL_SURFACE('',#4398,2.00000000000029);
#3866=CYLINDRICAL_SURFACE('',#4400,3.70283120062258);
#3867=CYLINDRICAL_SURFACE('',#4406,2.29663666580012);
#3868=CYLINDRICAL_SURFACE('',#4409,2.29663666580012);
#3869=CYLINDRICAL_SURFACE('',#4412,2.29663666580012);
#3870=CYLINDRICAL_SURFACE('',#4415,2.29663666580012);
#3871=CYLINDRICAL_SURFACE('',#4418,2.50000000000001);
#3872=CYLINDRICAL_SURFACE('',#4421,2.5);
#3873=CYLINDRICAL_SURFACE('',#4425,2.5);
#3874=CYLINDRICAL_SURFACE('',#4437,1.99475);
#3875=CYLINDRICAL_SURFACE('',#4439,1.99475);
#3876=CYLINDRICAL_SURFACE('',#4440,1.99475);
#3877=CYLINDRICAL_SURFACE('',#4441,1.99475);
#3878=CYLINDRICAL_SURFACE('',#4442,1.99475);
#3879=CYLINDRICAL_SURFACE('',#4443,1.99475);
#3880=CYLINDRICAL_SURFACE('',#4444,1.99475);
#3881=CYLINDRICAL_SURFACE('',#4445,1.99475);
#3882=CYLINDRICAL_SURFACE('',#4446,1.99475);
#3883=CYLINDRICAL_SURFACE('',#4447,1.99475);
#3884=CYLINDRICAL_SURFACE('',#4448,1.99475);
#3885=CYLINDRICAL_SURFACE('',#4449,1.99475);
#3886=CYLINDRICAL_SURFACE('',#4450,1.99475);
#3887=CYLINDRICAL_SURFACE('',#4451,1.99475);
#3888=CYLINDRICAL_SURFACE('',#4452,1.99475);
#3889=CYLINDRICAL_SURFACE('',#4453,1.99475);
#3890=CYLINDRICAL_SURFACE('',#4454,1.99475);
#3891=CYLINDRICAL_SURFACE('',#4455,1.99475);
#3892=CYLINDRICAL_SURFACE('',#4456,1.99475);
#3893=CYLINDRICAL_SURFACE('',#4457,1.99475);
#3894=CYLINDRICAL_SURFACE('',#4458,1.99475);
#3895=CYLINDRICAL_SURFACE('',#4459,1.99475);
#3896=CYLINDRICAL_SURFACE('',#4460,2.4505);
#3897=CYLINDRICAL_SURFACE('',#4463,1.99475);
#3898=CYLINDRICAL_SURFACE('',#4474,2.5);
#3899=CYLINDRICAL_SURFACE('',#4493,62.3332952479771);
#3900=CYLINDRICAL_SURFACE('',#4495,49.7730300598816);
#3901=CYLINDRICAL_SURFACE('',#4497,1.6332945980533);
#3902=CYLINDRICAL_SURFACE('',#4537,1.69478250292167);
#3903=CYLINDRICAL_SURFACE('',#4539,1.70133516896762);
#3904=CYLINDRICAL_SURFACE('',#4542,2.81236096609945);
#3905=CYLINDRICAL_SURFACE('',#4545,6.2515148621032);
#3906=CYLINDRICAL_SURFACE('',#4548,2.8615696413584);
#3907=CYLINDRICAL_SURFACE('',#4556,51.5001564610352);
#3908=CYLINDRICAL_SURFACE('',#4558,64.0604216491307);
#3909=CYLINDRICAL_SURFACE('',#4566,1.69478250292167);
#3910=CYLINDRICAL_SURFACE('',#4567,1.70133516896762);
#3911=CYLINDRICAL_SURFACE('',#4570,2.81236096609945);
#3912=CYLINDRICAL_SURFACE('',#4571,6.2515148621032);
#3913=CYLINDRICAL_SURFACE('',#4572,2.8615696413584);
#3914=CYLINDRICAL_SURFACE('',#4587,2.8615696413584);
#3915=CYLINDRICAL_SURFACE('',#4589,2.8615696413584);
#3916=CYLINDRICAL_SURFACE('',#4591,1.99589528357813);
#3917=CYLINDRICAL_SURFACE('',#4596,1.70133516896762);
#3918=CYLINDRICAL_SURFACE('',#4598,1.70133516896762);
#3919=CYLINDRICAL_SURFACE('',#4603,4.33051922028271);
#3920=CYLINDRICAL_SURFACE('',#4604,2.66551922028271);
#3921=CYLINDRICAL_SURFACE('',#4614,0.5);
#3922=CYLINDRICAL_SURFACE('',#4617,0.5);
#3923=CYLINDRICAL_SURFACE('',#4620,0.5);
#3924=CYLINDRICAL_SURFACE('',#4621,0.5);
#3925=CYLINDRICAL_SURFACE('',#4628,61.8868723549169);
#3926=CYLINDRICAL_SURFACE('',#4641,1.);
#3927=CYLINDRICAL_SURFACE('',#4652,1.);
#3928=CYLINDRICAL_SURFACE('',#4656,1.);
#3929=CYLINDRICAL_SURFACE('',#4660,62.3332952479768);
#3930=CYLINDRICAL_SURFACE('',#4664,19.7866355153418);
#3931=ADVANCED_FACE('',(#396),#3841,.F.);
#3932=ADVANCED_FACE('',(#397),#3842,.F.);
#3933=ADVANCED_FACE('',(#398),#3843,.T.);
#3934=ADVANCED_FACE('',(#399),#300,.T.);
#3935=ADVANCED_FACE('',(#400),#3844,.T.);
#3936=ADVANCED_FACE('',(#401),#301,.T.);
#3937=ADVANCED_FACE('',(#402,#265,#266),#302,.T.);
#3938=ADVANCED_FACE('',(#403,#267,#268),#303,.F.);
#3939=ADVANCED_FACE('',(#404),#213,.T.);
#3940=ADVANCED_FACE('',(#405),#304,.T.);
#3941=ADVANCED_FACE('',(#406),#214,.T.);
#3942=ADVANCED_FACE('',(#407),#305,.T.);
#3943=ADVANCED_FACE('',(#408),#3845,.F.);
#3944=ADVANCED_FACE('',(#409,#269,#270),#306,.T.);
#3945=ADVANCED_FACE('',(#410),#3846,.T.);
#3946=ADVANCED_FACE('',(#411),#307,.T.);
#3947=ADVANCED_FACE('',(#412),#3847,.T.);
#3948=ADVANCED_FACE('',(#413),#308,.F.);
#3949=ADVANCED_FACE('',(#414),#3848,.T.);
#3950=ADVANCED_FACE('',(#415),#309,.F.);
#3951=ADVANCED_FACE('',(#416),#3849,.T.);
#3952=ADVANCED_FACE('',(#417),#310,.F.);
#3953=ADVANCED_FACE('',(#418),#3850,.F.);
#3954=ADVANCED_FACE('',(#419),#311,.F.);
#3955=ADVANCED_FACE('',(#420),#3851,.F.);
#3956=ADVANCED_FACE('',(#421),#3852,.F.);
#3957=ADVANCED_FACE('',(#422),#312,.T.);
#3958=ADVANCED_FACE('',(#423),#313,.T.);
#3959=ADVANCED_FACE('',(#424),#314,.T.);
#3960=ADVANCED_FACE('',(#425),#315,.T.);
#3961=ADVANCED_FACE('',(#426),#3853,.F.);
#3962=ADVANCED_FACE('',(#427),#316,.T.);
#3963=ADVANCED_FACE('',(#428),#3854,.F.);
#3964=ADVANCED_FACE('',(#429),#317,.T.);
#3965=ADVANCED_FACE('',(#430),#3855,.F.);
#3966=ADVANCED_FACE('',(#431),#318,.T.);
#3967=ADVANCED_FACE('',(#432),#3856,.F.);
#3968=ADVANCED_FACE('',(#433),#319,.T.);
#3969=ADVANCED_FACE('',(#434),#3857,.T.);
#3970=ADVANCED_FACE('',(#435),#320,.T.);
#3971=ADVANCED_FACE('',(#436),#3858,.T.);
#3972=ADVANCED_FACE('',(#437,#271,#272),#321,.T.);
#3973=ADVANCED_FACE('',(#438,#273,#274),#322,.F.);
#3974=ADVANCED_FACE('',(#439),#215,.T.);
#3975=ADVANCED_FACE('',(#440),#323,.F.);
#3976=ADVANCED_FACE('',(#441),#216,.T.);
#3977=ADVANCED_FACE('',(#442),#324,.F.);
#3978=ADVANCED_FACE('',(#443),#3859,.F.);
#3979=ADVANCED_FACE('',(#444,#275,#276),#325,.F.);
#3980=ADVANCED_FACE('',(#445),#3860,.T.);
#3981=ADVANCED_FACE('',(#446),#326,.F.);
#3982=ADVANCED_FACE('',(#447,#277,#278),#327,.F.);
#3983=ADVANCED_FACE('',(#448),#3861,.T.);
#3984=ADVANCED_FACE('',(#449),#328,.T.);
#3985=ADVANCED_FACE('',(#450),#3862,.T.);
#3986=ADVANCED_FACE('',(#451),#329,.T.);
#3987=ADVANCED_FACE('',(#452),#3863,.T.);
#3988=ADVANCED_FACE('',(#453),#330,.T.);
#3989=ADVANCED_FACE('',(#454),#3864,.F.);
#3990=ADVANCED_FACE('',(#455),#331,.T.);
#3991=ADVANCED_FACE('',(#456),#3865,.F.);
#3992=ADVANCED_FACE('',(#457),#3866,.F.);
#3993=ADVANCED_FACE('',(#458),#332,.F.);
#3994=ADVANCED_FACE('',(#459),#333,.F.);
#3995=ADVANCED_FACE('',(#460),#334,.F.);
#3996=ADVANCED_FACE('',(#461),#335,.F.);
#3997=ADVANCED_FACE('',(#462),#3867,.F.);
#3998=ADVANCED_FACE('',(#463),#336,.F.);
#3999=ADVANCED_FACE('',(#464),#3868,.F.);
#4000=ADVANCED_FACE('',(#465),#337,.F.);
#4001=ADVANCED_FACE('',(#466),#3869,.F.);
#4002=ADVANCED_FACE('',(#467),#338,.F.);
#4003=ADVANCED_FACE('',(#468),#3870,.F.);
#4004=ADVANCED_FACE('',(#469),#339,.F.);
#4005=ADVANCED_FACE('',(#470),#3871,.T.);
#4006=ADVANCED_FACE('',(#471),#340,.F.);
#4007=ADVANCED_FACE('',(#472),#3872,.T.);
#4008=ADVANCED_FACE('',(#473,#279,#280),#341,.T.);
#4009=ADVANCED_FACE('',(#474),#3873,.F.);
#4010=ADVANCED_FACE('',(#475),#342,.T.);
#4011=ADVANCED_FACE('',(#476),#343,.T.);
#4012=ADVANCED_FACE('',(#477),#344,.T.);
#4013=ADVANCED_FACE('',(#478),#345,.T.);
#4014=ADVANCED_FACE('',(#479),#346,.T.);
#4015=ADVANCED_FACE('',(#480),#347,.T.);
#4016=ADVANCED_FACE('',(#481,#281),#348,.T.);
#4017=ADVANCED_FACE('',(#482,#282),#349,.F.);
#4018=ADVANCED_FACE('',(#483),#3874,.T.);
#4019=ADVANCED_FACE('',(#484),#3875,.T.);
#4020=ADVANCED_FACE('',(#485),#3876,.T.);
#4021=ADVANCED_FACE('',(#486),#3877,.T.);
#4022=ADVANCED_FACE('',(#487),#3878,.T.);
#4023=ADVANCED_FACE('',(#488),#3879,.T.);
#4024=ADVANCED_FACE('',(#489),#3880,.T.);
#4025=ADVANCED_FACE('',(#490),#3881,.T.);
#4026=ADVANCED_FACE('',(#491),#3882,.T.);
#4027=ADVANCED_FACE('',(#492),#3883,.T.);
#4028=ADVANCED_FACE('',(#493),#3884,.T.);
#4029=ADVANCED_FACE('',(#494),#3885,.T.);
#4030=ADVANCED_FACE('',(#495),#3886,.T.);
#4031=ADVANCED_FACE('',(#496),#3887,.T.);
#4032=ADVANCED_FACE('',(#497),#3888,.T.);
#4033=ADVANCED_FACE('',(#498),#3889,.T.);
#4034=ADVANCED_FACE('',(#499),#3890,.T.);
#4035=ADVANCED_FACE('',(#500),#3891,.T.);
#4036=ADVANCED_FACE('',(#501),#3892,.T.);
#4037=ADVANCED_FACE('',(#502),#3893,.T.);
#4038=ADVANCED_FACE('',(#503),#3894,.T.);
#4039=ADVANCED_FACE('',(#504),#3895,.T.);
#4040=ADVANCED_FACE('',(#505),#3896,.T.);
#4041=ADVANCED_FACE('',(#506),#3897,.T.);
#4042=ADVANCED_FACE('',(#507),#53,.F.);
#4043=ADVANCED_FACE('',(#508),#54,.F.);
#4044=ADVANCED_FACE('',(#509),#350,.T.);
#4045=ADVANCED_FACE('',(#510,#283),#351,.T.);
#4046=ADVANCED_FACE('',(#511),#51,.T.);
#4047=ADVANCED_FACE('',(#512),#52,.T.);
#4048=ADVANCED_FACE('',(#513),#352,.T.);
#4049=ADVANCED_FACE('',(#514),#3898,.F.);
#4050=ADVANCED_FACE('',(#515),#353,.T.);
#4051=ADVANCED_FACE('',(#516),#354,.T.);
#4052=ADVANCED_FACE('',(#517),#355,.T.);
#4053=ADVANCED_FACE('',(#518),#356,.T.);
#4054=ADVANCED_FACE('',(#519),#357,.T.);
#4055=ADVANCED_FACE('',(#520),#358,.T.);
#4056=ADVANCED_FACE('',(#521,#284),#359,.T.);
#4057=ADVANCED_FACE('',(#522,#285),#360,.F.);
#4058=ADVANCED_FACE('',(#523),#217,.T.);
#4059=ADVANCED_FACE('',(#524),#218,.T.);
#4060=ADVANCED_FACE('',(#525),#3899,.F.);
#4061=ADVANCED_FACE('',(#526),#3900,.F.);
#4062=ADVANCED_FACE('',(#527),#3901,.F.);
#4063=ADVANCED_FACE('',(#528),#219,.T.);
#4064=ADVANCED_FACE('',(#529),#220,.T.);
#4065=ADVANCED_FACE('',(#530,#286,#287),#361,.T.);
#4066=ADVANCED_FACE('',(#531),#362,.F.);
#4067=ADVANCED_FACE('',(#532),#221,.T.);
#4068=ADVANCED_FACE('',(#533),#363,.T.);
#4069=ADVANCED_FACE('',(#534),#364,.F.);
#4070=ADVANCED_FACE('',(#535),#222,.T.);
#4071=ADVANCED_FACE('',(#536),#365,.T.);
#4072=ADVANCED_FACE('',(#537),#366,.T.);
#4073=ADVANCED_FACE('',(#538),#223,.T.);
#4074=ADVANCED_FACE('',(#539),#367,.F.);
#4075=ADVANCED_FACE('',(#540),#368,.T.);
#4076=ADVANCED_FACE('',(#541),#224,.T.);
#4077=ADVANCED_FACE('',(#542),#369,.F.);
#4078=ADVANCED_FACE('',(#543),#3902,.F.);
#4079=ADVANCED_FACE('',(#544),#3903,.F.);
#4080=ADVANCED_FACE('',(#545),#370,.F.);
#4081=ADVANCED_FACE('',(#546),#55,.F.);
#4082=ADVANCED_FACE('',(#547),#3904,.T.);
#4083=ADVANCED_FACE('',(#548),#3905,.F.);
#4084=ADVANCED_FACE('',(#549),#3906,.T.);
#4085=ADVANCED_FACE('',(#550,#288,#289),#371,.F.);
#4086=ADVANCED_FACE('',(#551,#290,#291),#372,.T.);
#4087=ADVANCED_FACE('',(#552),#373,.T.);
#4088=ADVANCED_FACE('',(#553),#3907,.T.);
#4089=ADVANCED_FACE('',(#554),#3908,.T.);
#4090=ADVANCED_FACE('',(#555,#292,#293),#374,.F.);
#4091=ADVANCED_FACE('',(#556),#3909,.F.);
#4092=ADVANCED_FACE('',(#557),#3910,.F.);
#4093=ADVANCED_FACE('',(#558),#375,.T.);
#4094=ADVANCED_FACE('',(#559),#376,.T.);
#4095=ADVANCED_FACE('',(#560),#56,.T.);
#4096=ADVANCED_FACE('',(#561),#3911,.T.);
#4097=ADVANCED_FACE('',(#562),#3912,.F.);
#4098=ADVANCED_FACE('',(#563),#3913,.T.);
#4099=ADVANCED_FACE('',(#564),#57,.F.);
#4100=ADVANCED_FACE('',(#565),#58,.F.);
#4101=ADVANCED_FACE('',(#566,#294,#295),#377,.F.);
#4102=ADVANCED_FACE('',(#567),#378,.F.);
#4103=ADVANCED_FACE('',(#568),#379,.F.);
#4104=ADVANCED_FACE('',(#569),#380,.F.);
#4105=ADVANCED_FACE('',(#570),#59,.T.);
#4106=ADVANCED_FACE('',(#571,#296),#381,.F.);
#4107=ADVANCED_FACE('',(#572),#60,.F.);
#4108=ADVANCED_FACE('',(#573),#382,.F.);
#4109=ADVANCED_FACE('',(#574),#3914,.T.);
#4110=ADVANCED_FACE('',(#575),#3915,.T.);
#4111=ADVANCED_FACE('',(#576),#3916,.F.);
#4112=ADVANCED_FACE('',(#577,#297),#383,.F.);
#4113=ADVANCED_FACE('',(#578),#3917,.F.);
#4114=ADVANCED_FACE('',(#579),#3918,.F.);
#4115=ADVANCED_FACE('',(#580),#384,.T.);
#4116=ADVANCED_FACE('',(#581),#61,.T.);
#4117=ADVANCED_FACE('',(#582,#298,#299),#385,.T.);
#4118=ADVANCED_FACE('',(#583),#386,.T.);
#4119=ADVANCED_FACE('',(#584),#3919,.T.);
#4120=ADVANCED_FACE('',(#585),#3920,.F.);
#4121=ADVANCED_FACE('',(#586),#387,.T.);
#4122=ADVANCED_FACE('',(#587),#388,.T.);
#4123=ADVANCED_FACE('',(#588),#62,.F.);
#4124=ADVANCED_FACE('',(#589),#63,.F.);
#4125=ADVANCED_FACE('',(#590),#3921,.T.);
#4126=ADVANCED_FACE('',(#591),#64,.F.);
#4127=ADVANCED_FACE('',(#592),#3922,.T.);
#4128=ADVANCED_FACE('',(#593),#65,.F.);
#4129=ADVANCED_FACE('',(#594),#3923,.T.);
#4130=ADVANCED_FACE('',(#595),#3924,.T.);
#4131=ADVANCED_FACE('',(#596),#389,.F.);
#4132=ADVANCED_FACE('',(#597),#225,.T.);
#4133=ADVANCED_FACE('',(#598),#3925,.F.);
#4134=ADVANCED_FACE('',(#599),#226,.T.);
#4135=ADVANCED_FACE('',(#600),#390,.T.);
#4136=ADVANCED_FACE('',(#601),#66,.F.);
#4137=ADVANCED_FACE('',(#602),#47,.T.);
#4138=ADVANCED_FACE('',(#603),#227,.T.);
#4139=ADVANCED_FACE('',(#604),#3926,.T.);
#4140=ADVANCED_FACE('',(#605),#67,.F.);
#4141=ADVANCED_FACE('',(#606),#68,.T.);
#4142=ADVANCED_FACE('',(#607),#48,.T.);
#4143=ADVANCED_FACE('',(#608),#391,.T.);
#4144=ADVANCED_FACE('',(#609),#228,.T.);
#4145=ADVANCED_FACE('',(#610),#69,.F.);
#4146=ADVANCED_FACE('',(#611),#49,.T.);
#4147=ADVANCED_FACE('',(#612),#3927,.T.);
#4148=ADVANCED_FACE('',(#613),#50,.T.);
#4149=ADVANCED_FACE('',(#614),#3928,.T.);
#4150=ADVANCED_FACE('',(#615),#392,.T.);
#4151=ADVANCED_FACE('',(#616),#393,.T.);
#4152=ADVANCED_FACE('',(#617),#3929,.T.);
#4153=ADVANCED_FACE('',(#618),#394,.T.);
#4154=ADVANCED_FACE('',(#619),#70,.T.);
#4155=ADVANCED_FACE('',(#620),#395,.F.);
#4156=ADVANCED_FACE('',(#621),#3930,.T.);
#4157=CLOSED_SHELL('',(#3931,#3932,#3933,#3934,#3935,#3936,#3937,#3938));
#4158=CLOSED_SHELL('',(#3939,#3940,#3941,#3942,#3943,#3944,#3945,#3946,
#3947,#3948,#3949,#3950,#3951,#3952,#3953,#3954,#3955,#3956,#3957,#3958,
#3959,#3960,#3961,#3962,#3963,#3964,#3965,#3966,#3967,#3968,#3969,#3970,
#3971,#3972,#3973));
#4159=CLOSED_SHELL('',(#3974,#3975,#3976,#3977,#3978,#3979,#3980,#3981,
#3982,#3983,#3984,#3985,#3986,#3987,#3988,#3989,#3990,#3991,#3992,#3993,
#3994,#3995,#3996,#3997,#3998,#3999,#4000,#4001,#4002,#4003,#4004,#4005,
#4006,#4007,#4008));
#4160=CLOSED_SHELL('',(#4009,#4010,#4011,#4012,#4013,#4014,#4015,#4016,
#4017));
#4161=CLOSED_SHELL('',(#4018,#4019,#4020,#4021,#4022,#4023,#4024,#4025,
#4026,#4027,#4028,#4029,#4030,#4031,#4032,#4033,#4034,#4035,#4036,#4037,
#4038,#4039,#4040,#4041,#4042,#4043,#4044,#4045,#4046,#4047,#4048));
#4162=CLOSED_SHELL('',(#4049,#4050,#4051,#4052,#4053,#4054,#4055,#4056,
#4057));
#4163=CLOSED_SHELL('',(#4058,#4059,#4060,#4061,#4062,#4063,#4064,#4065,
#4066,#4067,#4068,#4069,#4070,#4071,#4072,#4073,#4074,#4075,#4076,#4077,
#4078,#4079,#4080,#4081,#4082,#4083,#4084,#4085,#4086,#4087,#4088,#4089,
#4090,#4091,#4092,#4093,#4094,#4095,#4096,#4097,#4098));
#4164=CLOSED_SHELL('',(#4099,#4100,#4101,#4102,#4103,#4104,#4105,#4106,
#4107,#4108,#4109,#4110,#4111,#4112,#4113,#4114,#4115,#4116,#4117,#4118,
#4119,#4120,#4121,#4122));
#4165=CLOSED_SHELL('',(#4123,#4124,#4125,#4126,#4127,#4128,#4129,#4130,
#4131,#4132,#4133,#4134,#4135,#4136,#4137,#4138,#4139,#4140,#4141,#4142,
#4143,#4144,#4145,#4146,#4147,#4148,#4149,#4150,#4151,#4152,#4153,#4154,
#4155,#4156));
#4166=DERIVED_UNIT_ELEMENT(#4184,1.);
#4167=DERIVED_UNIT_ELEMENT(#23579,-3.);
#4168=DERIVED_UNIT_ELEMENT(#4184,1.);
#4169=DERIVED_UNIT_ELEMENT(#23579,-3.);
#4170=DERIVED_UNIT_ELEMENT(#4184,1.);
#4171=DERIVED_UNIT_ELEMENT(#23579,-3.);
#4172=DERIVED_UNIT_ELEMENT(#4184,1.);
#4173=DERIVED_UNIT_ELEMENT(#23579,-3.);
#4174=DERIVED_UNIT_ELEMENT(#4184,1.);
#4175=DERIVED_UNIT_ELEMENT(#23579,-3.);
#4176=DERIVED_UNIT_ELEMENT(#4184,1.);
#4177=DERIVED_UNIT_ELEMENT(#23579,-3.);
#4178=DERIVED_UNIT_ELEMENT(#4184,1.);
#4179=DERIVED_UNIT_ELEMENT(#23579,-3.);
#4180=DERIVED_UNIT_ELEMENT(#4184,1.);
#4181=DERIVED_UNIT_ELEMENT(#23579,-3.);
#4182=DERIVED_UNIT_ELEMENT(#4184,1.);
#4183=DERIVED_UNIT_ELEMENT(#23579,-3.);
#4184=(
MASS_UNIT()
NAMED_UNIT(*)
SI_UNIT(.KILO.,.GRAM.)
);
#4185=DERIVED_UNIT((#4166,#4167));
#4186=DERIVED_UNIT((#4168,#4169));
#4187=DERIVED_UNIT((#4170,#4171));
#4188=DERIVED_UNIT((#4172,#4173));
#4189=DERIVED_UNIT((#4174,#4175));
#4190=DERIVED_UNIT((#4176,#4177));
#4191=DERIVED_UNIT((#4178,#4179));
#4192=DERIVED_UNIT((#4180,#4181));
#4193=DERIVED_UNIT((#4182,#4183));
#4194=MEASURE_REPRESENTATION_ITEM('density measure',
POSITIVE_RATIO_MEASURE(7850.),#4185);
#4195=MEASURE_REPRESENTATION_ITEM('density measure',
POSITIVE_RATIO_MEASURE(7850.),#4186);
#4196=MEASURE_REPRESENTATION_ITEM('density measure',
POSITIVE_RATIO_MEASURE(7850.),#4187);
#4197=MEASURE_REPRESENTATION_ITEM('density measure',
POSITIVE_RATIO_MEASURE(7850.),#4188);
#4198=MEASURE_REPRESENTATION_ITEM('density measure',
POSITIVE_RATIO_MEASURE(7850.),#4189);
#4199=MEASURE_REPRESENTATION_ITEM('density measure',
POSITIVE_RATIO_MEASURE(7850.),#4190);
#4200=MEASURE_REPRESENTATION_ITEM('density measure',
POSITIVE_RATIO_MEASURE(7850.),#4191);
#4201=MEASURE_REPRESENTATION_ITEM('density measure',
POSITIVE_RATIO_MEASURE(7850.),#4192);
#4202=MEASURE_REPRESENTATION_ITEM('density measure',
POSITIVE_RATIO_MEASURE(7850.),#4193);
#4203=PROPERTY_DEFINITION_REPRESENTATION(#4248,#4221);
#4204=PROPERTY_DEFINITION_REPRESENTATION(#4249,#4222);
#4205=PROPERTY_DEFINITION_REPRESENTATION(#4250,#4223);
#4206=PROPERTY_DEFINITION_REPRESENTATION(#4251,#4224);
#4207=PROPERTY_DEFINITION_REPRESENTATION(#4252,#4225);
#4208=PROPERTY_DEFINITION_REPRESENTATION(#4253,#4226);
#4209=PROPERTY_DEFINITION_REPRESENTATION(#4254,#4227);
#4210=PROPERTY_DEFINITION_REPRESENTATION(#4255,#4228);
#4211=PROPERTY_DEFINITION_REPRESENTATION(#4256,#4229);
#4212=PROPERTY_DEFINITION_REPRESENTATION(#4257,#4230);
#4213=PROPERTY_DEFINITION_REPRESENTATION(#4258,#4231);
#4214=PROPERTY_DEFINITION_REPRESENTATION(#4259,#4232);
#4215=PROPERTY_DEFINITION_REPRESENTATION(#4260,#4233);
#4216=PROPERTY_DEFINITION_REPRESENTATION(#4261,#4234);
#4217=PROPERTY_DEFINITION_REPRESENTATION(#4262,#4235);
#4218=PROPERTY_DEFINITION_REPRESENTATION(#4263,#4236);
#4219=PROPERTY_DEFINITION_REPRESENTATION(#4264,#4237);
#4220=PROPERTY_DEFINITION_REPRESENTATION(#4265,#4238);
#4221=REPRESENTATION('material name',(#4239),#23568);
#4222=REPRESENTATION('density',(#4194),#23568);
#4223=REPRESENTATION('material name',(#4240),#23569);
#4224=REPRESENTATION('density',(#4195),#23569);
#4225=REPRESENTATION('material name',(#4241),#23570);
#4226=REPRESENTATION('density',(#4196),#23570);
#4227=REPRESENTATION('material name',(#4242),#23571);
#4228=REPRESENTATION('density',(#4197),#23571);
#4229=REPRESENTATION('material name',(#4243),#23572);
#4230=REPRESENTATION('density',(#4198),#23572);
#4231=REPRESENTATION('material name',(#4244),#23573);
#4232=REPRESENTATION('density',(#4199),#23573);
#4233=REPRESENTATION('material name',(#4245),#23574);
#4234=REPRESENTATION('density',(#4200),#23574);
#4235=REPRESENTATION('material name',(#4246),#23575);
#4236=REPRESENTATION('density',(#4201),#23575);
#4237=REPRESENTATION('material name',(#4247),#23576);
#4238=REPRESENTATION('density',(#4202),#23576);
#4239=DESCRIPTIVE_REPRESENTATION_ITEM('Steel','Steel');
#4240=DESCRIPTIVE_REPRESENTATION_ITEM('Steel','Steel');
#4241=DESCRIPTIVE_REPRESENTATION_ITEM('Steel','Steel');
#4242=DESCRIPTIVE_REPRESENTATION_ITEM('Steel','Steel');
#4243=DESCRIPTIVE_REPRESENTATION_ITEM('Steel','Steel');
#4244=DESCRIPTIVE_REPRESENTATION_ITEM('Steel','Steel');
#4245=DESCRIPTIVE_REPRESENTATION_ITEM('Steel','Steel');
#4246=DESCRIPTIVE_REPRESENTATION_ITEM('Steel','Steel');
#4247=DESCRIPTIVE_REPRESENTATION_ITEM('Steel','Steel');
#4248=PROPERTY_DEFINITION('material property','material name',#23623);
#4249=PROPERTY_DEFINITION('material property','density of part',#23623);
#4250=PROPERTY_DEFINITION('material property','material name',#23624);
#4251=PROPERTY_DEFINITION('material property','density of part',#23624);
#4252=PROPERTY_DEFINITION('material property','material name',#23625);
#4253=PROPERTY_DEFINITION('material property','density of part',#23625);
#4254=PROPERTY_DEFINITION('material property','material name',#23626);
#4255=PROPERTY_DEFINITION('material property','density of part',#23626);
#4256=PROPERTY_DEFINITION('material property','material name',#23627);
#4257=PROPERTY_DEFINITION('material property','density of part',#23627);
#4258=PROPERTY_DEFINITION('material property','material name',#23628);
#4259=PROPERTY_DEFINITION('material property','density of part',#23628);
#4260=PROPERTY_DEFINITION('material property','material name',#23629);
#4261=PROPERTY_DEFINITION('material property','density of part',#23629);
#4262=PROPERTY_DEFINITION('material property','material name',#23630);
#4263=PROPERTY_DEFINITION('material property','density of part',#23630);
#4264=PROPERTY_DEFINITION('material property','material name',#23631);
#4265=PROPERTY_DEFINITION('material property','density of part',#23631);
#4266=AXIS2_PLACEMENT_3D('',#5775,#4674,#4675);
#4267=AXIS2_PLACEMENT_3D('',#5776,#4676,#4677);
#4268=AXIS2_PLACEMENT_3D('',#5777,#4678,#4679);
#4269=AXIS2_PLACEMENT_3D('',#5779,#4680,#4681);
#4270=AXIS2_PLACEMENT_3D('',#5782,#4683,#4684);
#4271=AXIS2_PLACEMENT_3D('',#5783,#4685,#4686);
#4272=AXIS2_PLACEMENT_3D('',#5785,#4687,#4688);
#4273=AXIS2_PLACEMENT_3D('',#5788,#4690,#4691);
#4274=AXIS2_PLACEMENT_3D('',#5789,#4692,#4693);
#4275=AXIS2_PLACEMENT_3D('',#5792,#4694,#4695);
#4276=AXIS2_PLACEMENT_3D('',#5796,#4697,#4698);
#4277=AXIS2_PLACEMENT_3D('',#5798,#4700,#4701);
#4278=AXIS2_PLACEMENT_3D('',#5804,#4705,#4706);
#4279=AXIS2_PLACEMENT_3D('',#5806,#4707,#4708);
#4280=AXIS2_PLACEMENT_3D('',#5808,#4709,#4710);
#4281=AXIS2_PLACEMENT_3D('',#5810,#4712,#4713);
#4282=AXIS2_PLACEMENT_3D('',#5813,#4716,#4717);
#4283=AXIS2_PLACEMENT_3D('',#5814,#4718,#4719);
#4284=AXIS2_PLACEMENT_3D('',#5815,#4720,#4721);
#4285=AXIS2_PLACEMENT_3D('',#5816,#4722,#4723);
#4286=AXIS2_PLACEMENT_3D('',#5818,#4724,#4725);
#4287=AXIS2_PLACEMENT_3D('',#5820,#4726,#4727);
#4288=AXIS2_PLACEMENT_3D('',#5821,#4728,#4729);
#4289=AXIS2_PLACEMENT_3D('',#5822,#4730,#4731);
#4290=AXIS2_PLACEMENT_3D('',#5823,#4732,#4733);
#4291=AXIS2_PLACEMENT_3D('',#5825,#4734,#4735);
#4292=AXIS2_PLACEMENT_3D('',#5827,#4736,#4737);
#4293=AXIS2_PLACEMENT_3D('',#5828,#4738,#4739);
#4294=AXIS2_PLACEMENT_3D('',#5829,#4740,#4741);
#4295=AXIS2_PLACEMENT_3D('',#5830,#4742,#4743);
#4296=AXIS2_PLACEMENT_3D('',#5833,#4744,#4745);
#4297=AXIS2_PLACEMENT_3D('',#5837,#4747,#4748);
#4298=AXIS2_PLACEMENT_3D('',#5839,#4750,#4751);
#4299=AXIS2_PLACEMENT_3D('',#5843,#4753,#4754);
#4300=AXIS2_PLACEMENT_3D('',#5847,#4756,#4757);
#4301=AXIS2_PLACEMENT_3D('',#5851,#4759,#4760);
#4302=AXIS2_PLACEMENT_3D('',#5853,#4761,#4762);
#4303=AXIS2_PLACEMENT_3D('',#5855,#4763,#4764);
#4304=AXIS2_PLACEMENT_3D('',#5859,#4766,#4767);
#4305=AXIS2_PLACEMENT_3D('',#5863,#4769,#4770);
#4306=AXIS2_PLACEMENT_3D('',#5865,#4772,#4773);
#4307=AXIS2_PLACEMENT_3D('',#5869,#4775,#4776);
#4308=AXIS2_PLACEMENT_3D('',#5871,#4778,#4779);
#4309=AXIS2_PLACEMENT_3D('',#5875,#4782,#4783);
#4310=AXIS2_PLACEMENT_3D('',#5878,#4784,#4785);
#4311=AXIS2_PLACEMENT_3D('',#5881,#4788,#4789);
#4312=AXIS2_PLACEMENT_3D('',#5885,#4792,#4793);
#4313=AXIS2_PLACEMENT_3D('',#5887,#4794,#4795);
#4314=AXIS2_PLACEMENT_3D('',#5889,#4797,#4798);
#4315=AXIS2_PLACEMENT_3D('',#5893,#4801,#4802);
#4316=AXIS2_PLACEMENT_3D('',#5897,#4804,#4805);
#4317=AXIS2_PLACEMENT_3D('',#5899,#4807,#4808);
#4318=AXIS2_PLACEMENT_3D('',#5903,#4811,#4812);
#4319=AXIS2_PLACEMENT_3D('',#5906,#4813,#4814);
#4320=AXIS2_PLACEMENT_3D('',#5909,#4817,#4818);
#4321=AXIS2_PLACEMENT_3D('',#5911,#4820,#4821);
#4322=AXIS2_PLACEMENT_3D('',#5913,#4822,#4823);
#4323=AXIS2_PLACEMENT_3D('',#5915,#4825,#4826);
#4324=AXIS2_PLACEMENT_3D('',#5916,#4827,#4828);
#4325=AXIS2_PLACEMENT_3D('',#5917,#4829,#4830);
#4326=AXIS2_PLACEMENT_3D('',#5925,#4835,#4836);
#4327=AXIS2_PLACEMENT_3D('',#5930,#4840,#4841);
#4328=AXIS2_PLACEMENT_3D('',#5931,#4842,#4843);
#4329=AXIS2_PLACEMENT_3D('',#5940,#4848,#4849);
#4330=AXIS2_PLACEMENT_3D('',#5942,#4850,#4851);
#4331=AXIS2_PLACEMENT_3D('',#5944,#4852,#4853);
#4332=AXIS2_PLACEMENT_3D('',#5946,#4855,#4856);
#4333=AXIS2_PLACEMENT_3D('',#5952,#4860,#4861);
#4334=AXIS2_PLACEMENT_3D('',#5953,#4862,#4863);
#4335=AXIS2_PLACEMENT_3D('',#5954,#4864,#4865);
#4336=AXIS2_PLACEMENT_3D('',#5955,#4866,#4867);
#4337=AXIS2_PLACEMENT_3D('',#5964,#4872,#4873);
#4338=AXIS2_PLACEMENT_3D('',#5966,#4874,#4875);
#4339=AXIS2_PLACEMENT_3D('',#5968,#4876,#4877);
#4340=AXIS2_PLACEMENT_3D('',#5970,#4879,#4880);
#4341=AXIS2_PLACEMENT_3D('',#5976,#4884,#4885);
#4342=AXIS2_PLACEMENT_3D('',#5977,#4886,#4887);
#4343=AXIS2_PLACEMENT_3D('',#5978,#4888,#4889);
#4344=AXIS2_PLACEMENT_3D('',#5979,#4890,#4891);
#4345=AXIS2_PLACEMENT_3D('',#5985,#4895,#4896);
#4346=AXIS2_PLACEMENT_3D('',#5987,#4897,#4898);
#4347=AXIS2_PLACEMENT_3D('',#5989,#4899,#4900);
#4348=AXIS2_PLACEMENT_3D('',#5991,#4902,#4903);
#4349=AXIS2_PLACEMENT_3D('',#5997,#4907,#4908);
#4350=AXIS2_PLACEMENT_3D('',#5998,#4909,#4910);
#4351=AXIS2_PLACEMENT_3D('',#5999,#4911,#4912);
#4352=AXIS2_PLACEMENT_3D('',#6000,#4913,#4914);
#4353=AXIS2_PLACEMENT_3D('',#6001,#4915,#4916);
#4354=AXIS2_PLACEMENT_3D('',#6002,#4917,#4918);
#4355=AXIS2_PLACEMENT_3D('',#6003,#4919,#4920);
#4356=AXIS2_PLACEMENT_3D('',#6005,#4921,#4922);
#4357=AXIS2_PLACEMENT_3D('',#6007,#4923,#4924);
#4358=AXIS2_PLACEMENT_3D('',#6008,#4925,#4926);
#4359=AXIS2_PLACEMENT_3D('',#6009,#4927,#4928);
#4360=AXIS2_PLACEMENT_3D('',#6010,#4929,#4930);
#4361=AXIS2_PLACEMENT_3D('',#6012,#4931,#4932);
#4362=AXIS2_PLACEMENT_3D('',#6014,#4933,#4934);
#4363=AXIS2_PLACEMENT_3D('',#6015,#4935,#4936);
#4364=AXIS2_PLACEMENT_3D('',#6016,#4937,#4938);
#4365=AXIS2_PLACEMENT_3D('',#6017,#4939,#4940);
#4366=AXIS2_PLACEMENT_3D('',#6020,#4941,#4942);
#4367=AXIS2_PLACEMENT_3D('',#6024,#4944,#4945);
#4368=AXIS2_PLACEMENT_3D('',#6026,#4947,#4948);
#4369=AXIS2_PLACEMENT_3D('',#6030,#4950,#4951);
#4370=AXIS2_PLACEMENT_3D('',#6034,#4953,#4954);
#4371=AXIS2_PLACEMENT_3D('',#6038,#4956,#4957);
#4372=AXIS2_PLACEMENT_3D('',#6042,#4959,#4960);
#4373=AXIS2_PLACEMENT_3D('',#6046,#4962,#4963);
#4374=AXIS2_PLACEMENT_3D('',#6050,#4965,#4966);
#4375=AXIS2_PLACEMENT_3D('',#6052,#4968,#4969);
#4376=AXIS2_PLACEMENT_3D('',#6055,#4970,#4971);
#4377=AXIS2_PLACEMENT_3D('',#6059,#4973,#4974);
#4378=AXIS2_PLACEMENT_3D('',#6061,#4976,#4977);
#4379=AXIS2_PLACEMENT_3D('',#6067,#4981,#4982);
#4380=AXIS2_PLACEMENT_3D('',#6071,#4984,#4985);
#4381=AXIS2_PLACEMENT_3D('',#6075,#4987,#4988);
#4382=AXIS2_PLACEMENT_3D('',#6079,#4990,#4991);
#4383=AXIS2_PLACEMENT_3D('',#6081,#4992,#4993);
#4384=AXIS2_PLACEMENT_3D('',#6083,#4994,#4995);
#4385=AXIS2_PLACEMENT_3D('',#6086,#4997,#4998);
#4386=AXIS2_PLACEMENT_3D('',#6088,#5000,#5001);
#4387=AXIS2_PLACEMENT_3D('',#6091,#5002,#5003);
#4388=AXIS2_PLACEMENT_3D('',#6094,#5006,#5007);
#4389=AXIS2_PLACEMENT_3D('',#6098,#5010,#5011);
#4390=AXIS2_PLACEMENT_3D('',#6100,#5012,#5013);
#4391=AXIS2_PLACEMENT_3D('',#6102,#5015,#5016);
#4392=AXIS2_PLACEMENT_3D('',#6106,#5019,#5020);
#4393=AXIS2_PLACEMENT_3D('',#6110,#5022,#5023);
#4394=AXIS2_PLACEMENT_3D('',#6112,#5025,#5026);
#4395=AXIS2_PLACEMENT_3D('',#6116,#5029,#5030);
#4396=AXIS2_PLACEMENT_3D('',#6119,#5031,#5032);
#4397=AXIS2_PLACEMENT_3D('',#6122,#5035,#5036);
#4398=AXIS2_PLACEMENT_3D('',#6124,#5038,#5039);
#4399=AXIS2_PLACEMENT_3D('',#6126,#5040,#5041);
#4400=AXIS2_PLACEMENT_3D('',#6128,#5043,#5044);
#4401=AXIS2_PLACEMENT_3D('',#6129,#5045,#5046);
#4402=AXIS2_PLACEMENT_3D('',#6130,#5047,#5048);
#4403=AXIS2_PLACEMENT_3D('',#6136,#5052,#5053);
#4404=AXIS2_PLACEMENT_3D('',#6141,#5057,#5058);
#4405=AXIS2_PLACEMENT_3D('',#6142,#5059,#5060);
#4406=AXIS2_PLACEMENT_3D('',#6148,#5064,#5065);
#4407=AXIS2_PLACEMENT_3D('',#6150,#5066,#5067);
#4408=AXIS2_PLACEMENT_3D('',#6152,#5069,#5070);
#4409=AXIS2_PLACEMENT_3D('',#6156,#5073,#5074);
#4410=AXIS2_PLACEMENT_3D('',#6157,#5075,#5076);
#4411=AXIS2_PLACEMENT_3D('',#6158,#5077,#5078);
#4412=AXIS2_PLACEMENT_3D('',#6164,#5082,#5083);
#4413=AXIS2_PLACEMENT_3D('',#6166,#5084,#5085);
#4414=AXIS2_PLACEMENT_3D('',#6168,#5087,#5088);
#4415=AXIS2_PLACEMENT_3D('',#6172,#5091,#5092);
#4416=AXIS2_PLACEMENT_3D('',#6173,#5093,#5094);
#4417=AXIS2_PLACEMENT_3D('',#6174,#5095,#5096);
#4418=AXIS2_PLACEMENT_3D('',#6178,#5099,#5100);
#4419=AXIS2_PLACEMENT_3D('',#6180,#5101,#5102);
#4420=AXIS2_PLACEMENT_3D('',#6182,#5104,#5105);
#4421=AXIS2_PLACEMENT_3D('',#6186,#5108,#5109);
#4422=AXIS2_PLACEMENT_3D('',#6187,#5110,#5111);
#4423=AXIS2_PLACEMENT_3D('',#6188,#5112,#5113);
#4424=AXIS2_PLACEMENT_3D('',#6189,#5114,#5115);
#4425=AXIS2_PLACEMENT_3D('',#6190,#5116,#5117);
#4426=AXIS2_PLACEMENT_3D('',#6192,#5118,#5119);
#4427=AXIS2_PLACEMENT_3D('',#6195,#5121,#5122);
#4428=AXIS2_PLACEMENT_3D('',#6196,#5123,#5124);
#4429=AXIS2_PLACEMENT_3D('',#6205,#5129,#5130);
#4430=AXIS2_PLACEMENT_3D('',#6211,#5134,#5135);
#4431=AXIS2_PLACEMENT_3D('',#6217,#5139,#5140);
#4432=AXIS2_PLACEMENT_3D('',#6223,#5144,#5145);
#4433=AXIS2_PLACEMENT_3D('',#6229,#5149,#5150);
#4434=AXIS2_PLACEMENT_3D('',#6232,#5153,#5154);
#4435=AXIS2_PLACEMENT_3D('',#6233,#5155,#5156);
#4436=AXIS2_PLACEMENT_3D('',#6234,#5157,#5158);
#4437=AXIS2_PLACEMENT_3D('',#6235,#5159,#5160);
#4438=AXIS2_PLACEMENT_3D('',#6441,#5162,#5163);
#4439=AXIS2_PLACEMENT_3D('',#6566,#5164,#5165);
#4440=AXIS2_PLACEMENT_3D('',#6796,#5167,#5168);
#4441=AXIS2_PLACEMENT_3D('',#7025,#5170,#5171);
#4442=AXIS2_PLACEMENT_3D('',#7438,#5173,#5174);
#4443=AXIS2_PLACEMENT_3D('',#7908,#5176,#5177);
#4444=AXIS2_PLACEMENT_3D('',#8398,#5179,#5180);
#4445=AXIS2_PLACEMENT_3D('',#8805,#5182,#5183);
#4446=AXIS2_PLACEMENT_3D('',#9040,#5185,#5186);
#4447=AXIS2_PLACEMENT_3D('',#9280,#5188,#5189);
#4448=AXIS2_PLACEMENT_3D('',#9766,#5191,#5192);
#4449=AXIS2_PLACEMENT_3D('',#10257,#5194,#5195);
#4450=AXIS2_PLACEMENT_3D('',#10683,#5197,#5198);
#4451=AXIS2_PLACEMENT_3D('',#11192,#5200,#5201);
#4452=AXIS2_PLACEMENT_3D('',#11676,#5203,#5204);
#4453=AXIS2_PLACEMENT_3D('',#11916,#5206,#5207);
#4454=AXIS2_PLACEMENT_3D('',#12149,#5209,#5210);
#4455=AXIS2_PLACEMENT_3D('',#12560,#5212,#5213);
#4456=AXIS2_PLACEMENT_3D('',#13022,#5215,#5216);
#4457=AXIS2_PLACEMENT_3D('',#13522,#5218,#5219);
#4458=AXIS2_PLACEMENT_3D('',#13935,#5221,#5222);
#4459=AXIS2_PLACEMENT_3D('',#14166,#5224,#5225);
#4460=AXIS2_PLACEMENT_3D('',#14396,#5227,#5228);
#4461=AXIS2_PLACEMENT_3D('',#14406,#5229,#5230);
#4462=AXIS2_PLACEMENT_3D('',#17019,#5231,#5232);
#4463=AXIS2_PLACEMENT_3D('',#19622,#5233,#5234);
#4464=AXIS2_PLACEMENT_3D('',#19825,#5235,#5236);
#4465=AXIS2_PLACEMENT_3D('',#21491,#5237,#5238);
#4466=AXIS2_PLACEMENT_3D('',#21492,#5239,#5240);
#4467=AXIS2_PLACEMENT_3D('',#21494,#5241,#5242);
#4468=AXIS2_PLACEMENT_3D('',#21495,#5243,#5244);
#4469=AXIS2_PLACEMENT_3D('',#21497,#5245,#5246);
#4470=AXIS2_PLACEMENT_3D('',#21499,#5248,#5249);
#4471=AXIS2_PLACEMENT_3D('',#21502,#5251,#5252);
#4472=AXIS2_PLACEMENT_3D('',#21503,#5253,#5254);
#4473=AXIS2_PLACEMENT_3D('',#21504,#5255,#5256);
#4474=AXIS2_PLACEMENT_3D('',#21505,#5257,#5258);
#4475=AXIS2_PLACEMENT_3D('',#21507,#5259,#5260);
#4476=AXIS2_PLACEMENT_3D('',#21510,#5262,#5263);
#4477=AXIS2_PLACEMENT_3D('',#21511,#5264,#5265);
#4478=AXIS2_PLACEMENT_3D('',#21520,#5270,#5271);
#4479=AXIS2_PLACEMENT_3D('',#21526,#5275,#5276);
#4480=AXIS2_PLACEMENT_3D('',#21532,#5280,#5281);
#4481=AXIS2_PLACEMENT_3D('',#21538,#5285,#5286);
#4482=AXIS2_PLACEMENT_3D('',#21544,#5290,#5291);
#4483=AXIS2_PLACEMENT_3D('',#21547,#5294,#5295);
#4484=AXIS2_PLACEMENT_3D('',#21548,#5296,#5297);
#4485=AXIS2_PLACEMENT_3D('',#21549,#5298,#5299);
#4486=AXIS2_PLACEMENT_3D('',#21550,#5300,#5301);
#4487=AXIS2_PLACEMENT_3D('',#21564,#5302,#5303);
#4488=AXIS2_PLACEMENT_3D('',#21566,#5304,#5305);
#4489=AXIS2_PLACEMENT_3D('',#21567,#5306,#5307);
#4490=AXIS2_PLACEMENT_3D('',#21568,#5308,#5309);
#4491=AXIS2_PLACEMENT_3D('',#21583,#5310,#5311);
#4492=AXIS2_PLACEMENT_3D('',#21584,#5312,#5313);
#4493=AXIS2_PLACEMENT_3D('',#21585,#5314,#5315);
#4494=AXIS2_PLACEMENT_3D('',#21589,#5317,#5318);
#4495=AXIS2_PLACEMENT_3D('',#21591,#5320,#5321);
#4496=AXIS2_PLACEMENT_3D('',#21594,#5323,#5324);
#4497=AXIS2_PLACEMENT_3D('',#21595,#5325,#5326);
#4498=AXIS2_PLACEMENT_3D('',#21597,#5327,#5328);
#4499=AXIS2_PLACEMENT_3D('',#21605,#5332,#5333);
#4500=AXIS2_PLACEMENT_3D('',#21618,#5334,#5335);
#4501=AXIS2_PLACEMENT_3D('',#21631,#5336,#5337);
#4502=AXIS2_PLACEMENT_3D('',#21632,#5338,#5339);
#4503=AXIS2_PLACEMENT_3D('',#21633,#5340,#5341);
#4504=AXIS2_PLACEMENT_3D('',#21634,#5342,#5343);
#4505=AXIS2_PLACEMENT_3D('',#21635,#5344,#5345);
#4506=AXIS2_PLACEMENT_3D('',#21639,#5347,#5348);
#4507=AXIS2_PLACEMENT_3D('',#21641,#5349,#5350);
#4508=AXIS2_PLACEMENT_3D('',#21643,#5351,#5352);
#4509=AXIS2_PLACEMENT_3D('',#21702,#5354,#5355);
#4510=AXIS2_PLACEMENT_3D('',#21704,#5356,#5357);
#4511=AXIS2_PLACEMENT_3D('',#21705,#5358,#5359);
#4512=AXIS2_PLACEMENT_3D('',#21707,#5360,#5361);
#4513=AXIS2_PLACEMENT_3D('',#21708,#5362,#5363);
#4514=AXIS2_PLACEMENT_3D('',#21710,#5364,#5365);
#4515=AXIS2_PLACEMENT_3D('',#21711,#5366,#5367);
#4516=AXIS2_PLACEMENT_3D('',#21712,#5368,#5369);
#4517=AXIS2_PLACEMENT_3D('',#21713,#5370,#5371);
#4518=AXIS2_PLACEMENT_3D('',#21715,#5372,#5373);
#4519=AXIS2_PLACEMENT_3D('',#21716,#5374,#5375);
#4520=AXIS2_PLACEMENT_3D('',#21718,#5376,#5377);
#4521=AXIS2_PLACEMENT_3D('',#21719,#5378,#5379);
#4522=AXIS2_PLACEMENT_3D('',#21720,#5380,#5381);
#4523=AXIS2_PLACEMENT_3D('',#21721,#5382,#5383);
#4524=AXIS2_PLACEMENT_3D('',#21723,#5384,#5385);
#4525=AXIS2_PLACEMENT_3D('',#21724,#5386,#5387);
#4526=AXIS2_PLACEMENT_3D('',#21726,#5388,#5389);
#4527=AXIS2_PLACEMENT_3D('',#21728,#5390,#5391);
#4528=AXIS2_PLACEMENT_3D('',#21729,#5392,#5393);
#4529=AXIS2_PLACEMENT_3D('',#21730,#5394,#5395);
#4530=AXIS2_PLACEMENT_3D('',#21731,#5396,#5397);
#4531=AXIS2_PLACEMENT_3D('',#21733,#5398,#5399);
#4532=AXIS2_PLACEMENT_3D('',#21734,#5400,#5401);
#4533=AXIS2_PLACEMENT_3D('',#21736,#5402,#5403);
#4534=AXIS2_PLACEMENT_3D('',#21738,#5404,#5405);
#4535=AXIS2_PLACEMENT_3D('',#21739,#5406,#5407);
#4536=AXIS2_PLACEMENT_3D('',#21740,#5408,#5409);
#4537=AXIS2_PLACEMENT_3D('',#21741,#5410,#5411);
#4538=AXIS2_PLACEMENT_3D('',#21744,#5413,#5414);
#4539=AXIS2_PLACEMENT_3D('',#21745,#5415,#5416);
#4540=AXIS2_PLACEMENT_3D('',#21748,#5418,#5419);
#4541=AXIS2_PLACEMENT_3D('',#21749,#5420,#5421);
#4542=AXIS2_PLACEMENT_3D('',#21981,#5427,#5428);
#4543=AXIS2_PLACEMENT_3D('',#21983,#5429,#5430);
#4544=AXIS2_PLACEMENT_3D('',#21986,#5432,#5433);
#4545=AXIS2_PLACEMENT_3D('',#21987,#5434,#5435);
#4546=AXIS2_PLACEMENT_3D('',#21989,#5436,#5437);
#4547=AXIS2_PLACEMENT_3D('',#21992,#5439,#5440);
#4548=AXIS2_PLACEMENT_3D('',#21993,#5441,#5442);
#4549=AXIS2_PLACEMENT_3D('',#21994,#5443,#5444);
#4550=AXIS2_PLACEMENT_3D('',#21995,#5445,#5446);
#4551=AXIS2_PLACEMENT_3D('',#21996,#5447,#5448);
#4552=AXIS2_PLACEMENT_3D('',#21998,#5450,#5451);
#4553=AXIS2_PLACEMENT_3D('',#22004,#5454,#5455);
#4554=AXIS2_PLACEMENT_3D('',#22005,#5456,#5457);
#4555=AXIS2_PLACEMENT_3D('',#22006,#5458,#5459);
#4556=AXIS2_PLACEMENT_3D('',#22010,#5462,#5463);
#4557=AXIS2_PLACEMENT_3D('',#22013,#5465,#5466);
#4558=AXIS2_PLACEMENT_3D('',#22014,#5467,#5468);
#4559=AXIS2_PLACEMENT_3D('',#22017,#5470,#5471);
#4560=AXIS2_PLACEMENT_3D('',#22018,#5472,#5473);
#4561=AXIS2_PLACEMENT_3D('',#22078,#5475,#5476);
#4562=AXIS2_PLACEMENT_3D('',#22080,#5477,#5478);
#4563=AXIS2_PLACEMENT_3D('',#22082,#5479,#5480);
#4564=AXIS2_PLACEMENT_3D('',#22085,#5482,#5483);
#4565=AXIS2_PLACEMENT_3D('',#22087,#5484,#5485);
#4566=AXIS2_PLACEMENT_3D('',#22088,#5486,#5487);
#4567=AXIS2_PLACEMENT_3D('',#22090,#5489,#5490);
#4568=AXIS2_PLACEMENT_3D('',#22092,#5492,#5493);
#4569=AXIS2_PLACEMENT_3D('',#22094,#5495,#5496);
#4570=AXIS2_PLACEMENT_3D('',#22207,#5499,#5500);
#4571=AXIS2_PLACEMENT_3D('',#22209,#5502,#5503);
#4572=AXIS2_PLACEMENT_3D('',#22211,#5505,#5506);
#4573=AXIS2_PLACEMENT_3D('',#22212,#5507,#5508);
#4574=AXIS2_PLACEMENT_3D('',#22365,#5513,#5514);
#4575=AXIS2_PLACEMENT_3D('',#22368,#5515,#5516);
#4576=AXIS2_PLACEMENT_3D('',#22396,#5520,#5521);
#4577=AXIS2_PLACEMENT_3D('',#22398,#5522,#5523);
#4578=AXIS2_PLACEMENT_3D('',#22401,#5525,#5526);
#4579=AXIS2_PLACEMENT_3D('',#22403,#5527,#5528);
#4580=AXIS2_PLACEMENT_3D('',#22404,#5529,#5530);
#4581=AXIS2_PLACEMENT_3D('',#22410,#5534,#5535);
#4582=AXIS2_PLACEMENT_3D('',#22419,#5540,#5541);
#4583=AXIS2_PLACEMENT_3D('',#22485,#5545,#5546);
#4584=AXIS2_PLACEMENT_3D('',#22513,#5550,#5551);
#4585=AXIS2_PLACEMENT_3D('',#22515,#5552,#5553);
#4586=AXIS2_PLACEMENT_3D('',#22581,#5557,#5558);
#4587=AXIS2_PLACEMENT_3D('',#22585,#5561,#5562);
#4588=AXIS2_PLACEMENT_3D('',#22588,#5564,#5565);
#4589=AXIS2_PLACEMENT_3D('',#22589,#5566,#5567);
#4590=AXIS2_PLACEMENT_3D('',#22593,#5569,#5570);
#4591=AXIS2_PLACEMENT_3D('',#22595,#5572,#5573);
#4592=AXIS2_PLACEMENT_3D('',#22598,#5575,#5576);
#4593=AXIS2_PLACEMENT_3D('',#22599,#5577,#5578);
#4594=AXIS2_PLACEMENT_3D('',#22601,#5579,#5580);
#4595=AXIS2_PLACEMENT_3D('',#22630,#5585,#5586);
#4596=AXIS2_PLACEMENT_3D('',#22631,#5587,#5588);
#4597=AXIS2_PLACEMENT_3D('',#22633,#5589,#5590);
#4598=AXIS2_PLACEMENT_3D('',#22635,#5592,#5593);
#4599=AXIS2_PLACEMENT_3D('',#22637,#5594,#5595);
#4600=AXIS2_PLACEMENT_3D('',#22639,#5597,#5598);
#4601=AXIS2_PLACEMENT_3D('',#22683,#5602,#5603);
#4602=AXIS2_PLACEMENT_3D('',#22684,#5604,#5605);
#4603=AXIS2_PLACEMENT_3D('',#22686,#5607,#5608);
#4604=AXIS2_PLACEMENT_3D('',#22687,#5609,#5610);
#4605=AXIS2_PLACEMENT_3D('',#22689,#5612,#5613);
#4606=AXIS2_PLACEMENT_3D('',#22691,#5615,#5616);
#4607=AXIS2_PLACEMENT_3D('',#22692,#5617,#5618);
#4608=AXIS2_PLACEMENT_3D('',#22731,#5619,#5620);
#4609=AXIS2_PLACEMENT_3D('',#22774,#5621,#5622);
#4610=AXIS2_PLACEMENT_3D('',#22782,#5623,#5624);
#4611=AXIS2_PLACEMENT_3D('',#22821,#5625,#5626);
#4612=AXIS2_PLACEMENT_3D('',#22864,#5627,#5628);
#4613=AXIS2_PLACEMENT_3D('',#22866,#5629,#5630);
#4614=AXIS2_PLACEMENT_3D('',#22873,#5631,#5632);
#4615=AXIS2_PLACEMENT_3D('',#22876,#5633,#5634);
#4616=AXIS2_PLACEMENT_3D('',#22911,#5637,#5638);
#4617=AXIS2_PLACEMENT_3D('',#22924,#5639,#5640);
#4618=AXIS2_PLACEMENT_3D('',#22927,#5641,#5642);
#4619=AXIS2_PLACEMENT_3D('',#22957,#5645,#5646);
#4620=AXIS2_PLACEMENT_3D('',#22968,#5647,#5648);
#4621=AXIS2_PLACEMENT_3D('',#22971,#5651,#5652);
#4622=AXIS2_PLACEMENT_3D('',#22974,#5655,#5656);
#4623=AXIS2_PLACEMENT_3D('',#22976,#5657,#5658);
#4624=AXIS2_PLACEMENT_3D('',#22990,#5660,#5661);
#4625=AXIS2_PLACEMENT_3D('',#22991,#5662,#5663);
#4626=AXIS2_PLACEMENT_3D('',#22993,#5664,#5665);
#4627=AXIS2_PLACEMENT_3D('',#22994,#5666,#5667);
#4628=AXIS2_PLACEMENT_3D('',#22995,#5668,#5669);
#4629=AXIS2_PLACEMENT_3D('',#22997,#5670,#5671);
#4630=AXIS2_PLACEMENT_3D('',#22999,#5673,#5674);
#4631=AXIS2_PLACEMENT_3D('',#23001,#5675,#5676);
#4632=AXIS2_PLACEMENT_3D('',#23002,#5677,#5678);
#4633=AXIS2_PLACEMENT_3D('',#23003,#5679,#5680);
#4634=AXIS2_PLACEMENT_3D('',#23076,#5684,#5685);
#4635=AXIS2_PLACEMENT_3D('',#23105,#5686,#5687);
#4636=AXIS2_PLACEMENT_3D('',#23107,#5688,#5689);
#4637=AXIS2_PLACEMENT_3D('',#23108,#5690,#5691);
#4638=AXIS2_PLACEMENT_3D('',#23109,#5692,#5693);
#4639=AXIS2_PLACEMENT_3D('',#23110,#5694,#5695);
#4640=AXIS2_PLACEMENT_3D('',#23111,#5696,#5697);
#4641=AXIS2_PLACEMENT_3D('',#23112,#5698,#5699);
#4642=AXIS2_PLACEMENT_3D('',#23115,#5701,#5702);
#4643=AXIS2_PLACEMENT_3D('',#23130,#5705,#5706);
#4644=AXIS2_PLACEMENT_3D('',#23193,#5709,#5710);
#4645=AXIS2_PLACEMENT_3D('',#23194,#5711,#5712);
#4646=AXIS2_PLACEMENT_3D('',#23195,#5713,#5714);
#4647=AXIS2_PLACEMENT_3D('',#23196,#5715,#5716);
#4648=AXIS2_PLACEMENT_3D('',#23213,#5717,#5718);
#4649=AXIS2_PLACEMENT_3D('',#23264,#5719,#5720);
#4650=AXIS2_PLACEMENT_3D('',#23265,#5721,#5722);
#4651=AXIS2_PLACEMENT_3D('',#23266,#5723,#5724);
#4652=AXIS2_PLACEMENT_3D('',#23267,#5725,#5726);
#4653=AXIS2_PLACEMENT_3D('',#23269,#5727,#5728);
#4654=AXIS2_PLACEMENT_3D('',#23271,#5730,#5731);
#4655=AXIS2_PLACEMENT_3D('',#23272,#5732,#5733);
#4656=AXIS2_PLACEMENT_3D('',#23273,#5734,#5735);
#4657=AXIS2_PLACEMENT_3D('',#23275,#5737,#5738);
#4658=AXIS2_PLACEMENT_3D('',#23276,#5739,#5740);
#4659=AXIS2_PLACEMENT_3D('',#23437,#5742,#5743);
#4660=AXIS2_PLACEMENT_3D('',#23438,#5744,#5745);
#4661=AXIS2_PLACEMENT_3D('',#23441,#5747,#5748);
#4662=AXIS2_PLACEMENT_3D('',#23442,#5749,#5750);
#4663=AXIS2_PLACEMENT_3D('',#23545,#5753,#5754);
#4664=AXIS2_PLACEMENT_3D('',#23546,#5755,#5756);
#4665=AXIS2_PLACEMENT_3D('',#23547,#5757,#5758);
#4666=AXIS2_PLACEMENT_3D('',#23548,#5759,#5760);
#4667=AXIS2_PLACEMENT_3D('',#23549,#5761,#5762);
#4668=AXIS2_PLACEMENT_3D('',#23550,#5763,#5764);
#4669=AXIS2_PLACEMENT_3D('',#23551,#5765,#5766);
#4670=AXIS2_PLACEMENT_3D('',#23552,#5767,#5768);
#4671=AXIS2_PLACEMENT_3D('',#23553,#5769,#5770);
#4672=AXIS2_PLACEMENT_3D('',#23554,#5771,#5772);
#4673=AXIS2_PLACEMENT_3D('',#23555,#5773,#5774);
#4674=DIRECTION('axis',(0.,0.,1.));
#4675=DIRECTION('refdir',(1.,0.,0.));
#4676=DIRECTION('axis',(0.,0.,1.));
#4677=DIRECTION('refdir',(1.,0.,0.));
#4678=DIRECTION('center_axis',(0.,-1.,0.));
#4679=DIRECTION('ref_axis',(1.,0.,0.));
#4680=DIRECTION('center_axis',(0.,1.,0.));
#4681=DIRECTION('ref_axis',(1.,0.,0.));
#4682=DIRECTION('',(0.,-1.,0.));
#4683=DIRECTION('center_axis',(0.,1.,0.));
#4684=DIRECTION('ref_axis',(1.,0.,0.));
#4685=DIRECTION('center_axis',(0.,-1.,0.));
#4686=DIRECTION('ref_axis',(1.,0.,0.));
#4687=DIRECTION('center_axis',(0.,1.,0.));
#4688=DIRECTION('ref_axis',(1.,0.,0.));
#4689=DIRECTION('',(0.,-1.,0.));
#4690=DIRECTION('center_axis',(0.,1.,0.));
#4691=DIRECTION('ref_axis',(1.,0.,0.));
#4692=DIRECTION('center_axis',(0.,-1.,0.));
#4693=DIRECTION('ref_axis',(1.,0.,0.));
#4694=DIRECTION('center_axis',(0.,-1.,0.));
#4695=DIRECTION('ref_axis',(1.,0.,0.));
#4696=DIRECTION('',(0.,-1.,0.));
#4697=DIRECTION('center_axis',(0.,-1.,0.));
#4698=DIRECTION('ref_axis',(1.,0.,0.));
#4699=DIRECTION('',(0.,-1.,0.));
#4700=DIRECTION('center_axis',(-0.519736754180336,0.,-0.854326463568869));
#4701=DIRECTION('ref_axis',(0.854326463568869,8.60567687699182E-17,-0.519736754180336));
#4702=DIRECTION('',(0.854326463568868,8.60567687699182E-17,-0.519736754180336));
#4703=DIRECTION('',(0.854326463568868,8.60567687699182E-17,-0.519736754180336));
#4704=DIRECTION('',(0.,-1.,0.));
#4705=DIRECTION('center_axis',(0.,-1.,0.));
#4706=DIRECTION('ref_axis',(-0.805071965104942,0.,0.593177149763936));
#4707=DIRECTION('center_axis',(0.,-1.,0.));
#4708=DIRECTION('ref_axis',(1.,0.,0.));
#4709=DIRECTION('center_axis',(0.,-1.,0.));
#4710=DIRECTION('ref_axis',(1.,0.,0.));
#4711=DIRECTION('',(0.,-1.,0.));
#4712=DIRECTION('center_axis',(0.632123897156508,0.,0.774867329704685));
#4713=DIRECTION('ref_axis',(-0.774867329704685,-9.00832757384467E-17,0.632123897156508));
#4714=DIRECTION('',(-0.774867329704685,-9.00832757384467E-17,0.632123897156508));
#4715=DIRECTION('',(-0.774867329704685,-9.00832757384467E-17,0.632123897156508));
#4716=DIRECTION('center_axis',(0.,-1.,0.));
#4717=DIRECTION('ref_axis',(1.,0.,0.));
#4718=DIRECTION('center_axis',(0.,-1.,0.));
#4719=DIRECTION('ref_axis',(1.,0.,0.));
#4720=DIRECTION('axis',(0.,0.,1.));
#4721=DIRECTION('refdir',(1.,0.,0.));
#4722=DIRECTION('center_axis',(0.,-1.,0.));
#4723=DIRECTION('ref_axis',(0.,0.,-1.));
#4724=DIRECTION('center_axis',(0.,1.,0.));
#4725=DIRECTION('ref_axis',(1.,0.,0.));
#4726=DIRECTION('center_axis',(-1.,0.,0.));
#4727=DIRECTION('ref_axis',(0.,0.,1.));
#4728=DIRECTION('center_axis',(0.,1.,0.));
#4729=DIRECTION('ref_axis',(0.,0.,-1.));
#4730=DIRECTION('center_axis',(0.,-1.,0.));
#4731=DIRECTION('ref_axis',(1.,0.,0.));
#4732=DIRECTION('center_axis',(0.,-1.,0.));
#4733=DIRECTION('ref_axis',(0.,0.,-1.));
#4734=DIRECTION('center_axis',(0.,1.,0.));
#4735=DIRECTION('ref_axis',(1.,0.,0.));
#4736=DIRECTION('center_axis',(-1.,0.,0.));
#4737=DIRECTION('ref_axis',(0.,0.,1.));
#4738=DIRECTION('center_axis',(0.,1.,0.));
#4739=DIRECTION('ref_axis',(0.,0.,-1.));
#4740=DIRECTION('center_axis',(0.,-1.,0.));
#4741=DIRECTION('ref_axis',(1.,0.,0.));
#4742=DIRECTION('center_axis',(-1.,0.,0.));
#4743=DIRECTION('ref_axis',(0.,0.707106781186547,-0.707106781186548));
#4744=DIRECTION('center_axis',(-0.924850298995146,0.,0.380331335086382));
#4745=DIRECTION('ref_axis',(-0.380331335086382,-3.4226336542529E-16,-0.924850298995146));
#4746=DIRECTION('',(1.,0.,0.));
#4747=DIRECTION('center_axis',(0.924850298995146,0.,0.380331335086382));
#4748=DIRECTION('ref_axis',(0.380331335086382,0.,-0.924850298995146));
#4749=DIRECTION('',(-1.,0.,0.));
#4750=DIRECTION('center_axis',(0.,-1.,0.));
#4751=DIRECTION('ref_axis',(1.,0.,0.));
#4752=DIRECTION('',(-0.380331335086382,0.,0.924850298995146));
#4753=DIRECTION('center_axis',(0.,1.,0.));
#4754=DIRECTION('ref_axis',(0.556627642555425,0.,0.830762100449455));
#4755=DIRECTION('',(1.,0.,0.));
#4756=DIRECTION('center_axis',(0.,1.,0.));
#4757=DIRECTION('ref_axis',(-0.707106781186548,0.,0.707106781186548));
#4758=DIRECTION('',(0.,0.,-1.));
#4759=DIRECTION('center_axis',(0.,1.,0.));
#4760=DIRECTION('ref_axis',(0.965748659616483,0.,-0.259479337229319));
#4761=DIRECTION('center_axis',(0.,1.,0.));
#4762=DIRECTION('ref_axis',(-0.965748659616478,0.,-0.259479337229339));
#4763=DIRECTION('center_axis',(0.,1.,0.));
#4764=DIRECTION('ref_axis',(-1.,0.,-1.85962356624686E-14));
#4765=DIRECTION('',(0.,0.,1.));
#4766=DIRECTION('center_axis',(0.,1.,0.));
#4767=DIRECTION('ref_axis',(0.707106781186548,0.,0.707106781186548));
#4768=DIRECTION('',(1.,0.,0.));
#4769=DIRECTION('center_axis',(0.,1.,0.));
#4770=DIRECTION('ref_axis',(-0.556627642555424,0.,0.830762100449455));
#4771=DIRECTION('',(-0.380331335086382,0.,-0.924850298995146));
#4772=DIRECTION('center_axis',(0.,-1.,0.));
#4773=DIRECTION('ref_axis',(-0.707106781186548,0.,0.707106781186548));
#4774=DIRECTION('',(0.,1.,0.));
#4775=DIRECTION('center_axis',(0.,-1.,0.));
#4776=DIRECTION('ref_axis',(-0.707106781186548,0.,0.707106781186548));
#4777=DIRECTION('',(0.,-1.,0.));
#4778=DIRECTION('center_axis',(0.,0.,1.));
#4779=DIRECTION('ref_axis',(1.,0.,0.));
#4780=DIRECTION('',(0.,-1.,0.));
#4781=DIRECTION('',(-1.,0.,0.));
#4782=DIRECTION('center_axis',(0.,1.,0.));
#4783=DIRECTION('ref_axis',(0.707106781186548,0.,0.707106781186548));
#4784=DIRECTION('center_axis',(0.,-1.,0.));
#4785=DIRECTION('ref_axis',(0.707106781186548,0.,0.707106781186548));
#4786=DIRECTION('',(0.,-1.,0.));
#4787=DIRECTION('',(0.,1.,0.));
#4788=DIRECTION('center_axis',(-1.,0.,0.));
#4789=DIRECTION('ref_axis',(0.,0.,1.));
#4790=DIRECTION('',(0.,1.,0.));
#4791=DIRECTION('',(0.,0.,-1.));
#4792=DIRECTION('center_axis',(0.,1.,0.));
#4793=DIRECTION('ref_axis',(0.556627642555425,0.,0.830762100449455));
#4794=DIRECTION('center_axis',(0.,-1.,0.));
#4795=DIRECTION('ref_axis',(0.556627642555425,0.,0.830762100449455));
#4796=DIRECTION('',(0.,1.,0.));
#4797=DIRECTION('center_axis',(-0.924850298995146,0.,-0.380331335086382));
#4798=DIRECTION('ref_axis',(-0.380331335086382,0.,0.924850298995145));
#4799=DIRECTION('',(0.,1.,0.));
#4800=DIRECTION('',(0.380331335086382,0.,-0.924850298995146));
#4801=DIRECTION('center_axis',(0.,-1.,0.));
#4802=DIRECTION('ref_axis',(-0.556627642555424,0.,0.830762100449455));
#4803=DIRECTION('',(0.,1.,0.));
#4804=DIRECTION('center_axis',(0.,-1.,0.));
#4805=DIRECTION('ref_axis',(-0.556627642555424,0.,0.830762100449455));
#4806=DIRECTION('',(0.,-1.,0.));
#4807=DIRECTION('center_axis',(0.924850298995146,0.,-0.380331335086382));
#4808=DIRECTION('ref_axis',(-0.380331335086382,0.,-0.924850298995145));
#4809=DIRECTION('',(0.380331335086382,0.,0.924850298995146));
#4810=DIRECTION('',(3.51417407375166E-16,-1.,0.));
#4811=DIRECTION('center_axis',(0.,1.,0.));
#4812=DIRECTION('ref_axis',(0.965748659616483,0.,-0.259479337229319));
#4813=DIRECTION('center_axis',(0.,-1.,0.));
#4814=DIRECTION('ref_axis',(0.965748659616483,0.,-0.259479337229319));
#4815=DIRECTION('',(0.,1.,0.));
#4816=DIRECTION('',(0.,1.,0.));
#4817=DIRECTION('center_axis',(1.,0.,0.));
#4818=DIRECTION('ref_axis',(0.,0.,-1.));
#4819=DIRECTION('',(0.,0.,1.));
#4820=DIRECTION('center_axis',(0.,1.,0.));
#4821=DIRECTION('ref_axis',(-1.,0.,-1.85962356624686E-14));
#4822=DIRECTION('center_axis',(0.,-1.,0.));
#4823=DIRECTION('ref_axis',(-1.,0.,-1.85962356624686E-14));
#4824=DIRECTION('',(0.,1.,0.));
#4825=DIRECTION('center_axis',(0.,1.,0.));
#4826=DIRECTION('ref_axis',(-0.965748659616478,0.,-0.259479337229339));
#4827=DIRECTION('center_axis',(0.,-1.,0.));
#4828=DIRECTION('ref_axis',(-0.965748659616478,0.,-0.259479337229339));
#4829=DIRECTION('center_axis',(1.,0.,0.));
#4830=DIRECTION('ref_axis',(0.,1.,0.));
#4831=DIRECTION('',(0.,1.,0.));
#4832=DIRECTION('',(0.,0.,1.));
#4833=DIRECTION('',(0.,-1.,0.));
#4834=DIRECTION('',(0.,0.,1.));
#4835=DIRECTION('center_axis',(0.,1.,0.));
#4836=DIRECTION('ref_axis',(-1.,0.,0.));
#4837=DIRECTION('',(-1.,0.,0.));
#4838=DIRECTION('',(0.,0.,1.));
#4839=DIRECTION('',(-1.,0.,0.));
#4840=DIRECTION('center_axis',(0.,0.,1.));
#4841=DIRECTION('ref_axis',(1.,0.,0.));
#4842=DIRECTION('center_axis',(0.,1.,0.));
#4843=DIRECTION('ref_axis',(-1.,0.,0.));
#4844=DIRECTION('',(-1.,0.,0.));
#4845=DIRECTION('',(0.,0.,1.));
#4846=DIRECTION('',(-1.,0.,0.));
#4847=DIRECTION('',(0.,0.,1.));
#4848=DIRECTION('center_axis',(0.,0.,1.));
#4849=DIRECTION('ref_axis',(0.,-1.,0.));
#4850=DIRECTION('center_axis',(0.,0.,-1.));
#4851=DIRECTION('ref_axis',(0.,-1.,0.));
#4852=DIRECTION('center_axis',(0.,0.,-1.));
#4853=DIRECTION('ref_axis',(0.,-1.,0.));
#4854=DIRECTION('',(0.,0.,1.));
#4855=DIRECTION('center_axis',(0.,-1.,0.));
#4856=DIRECTION('ref_axis',(1.,0.,0.));
#4857=DIRECTION('',(1.,0.,0.));
#4858=DIRECTION('',(1.,0.,0.));
#4859=DIRECTION('',(0.,0.,1.));
#4860=DIRECTION('center_axis',(0.,0.,1.));
#4861=DIRECTION('ref_axis',(0.,1.,0.));
#4862=DIRECTION('center_axis',(0.,0.,-1.));
#4863=DIRECTION('ref_axis',(0.,1.,0.));
#4864=DIRECTION('center_axis',(0.,0.,-1.));
#4865=DIRECTION('ref_axis',(0.,1.,0.));
#4866=DIRECTION('center_axis',(0.,1.,0.));
#4867=DIRECTION('ref_axis',(-1.,0.,0.));
#4868=DIRECTION('',(-1.,0.,0.));
#4869=DIRECTION('',(0.,0.,1.));
#4870=DIRECTION('',(-1.,0.,0.));
#4871=DIRECTION('',(0.,0.,1.));
#4872=DIRECTION('center_axis',(0.,0.,1.));
#4873=DIRECTION('ref_axis',(0.,-1.,0.));
#4874=DIRECTION('center_axis',(0.,0.,-1.));
#4875=DIRECTION('ref_axis',(0.,-1.,0.));
#4876=DIRECTION('center_axis',(0.,0.,-1.));
#4877=DIRECTION('ref_axis',(0.,-1.,0.));
#4878=DIRECTION('',(0.,0.,1.));
#4879=DIRECTION('center_axis',(0.,-1.,0.));
#4880=DIRECTION('ref_axis',(1.,0.,0.));
#4881=DIRECTION('',(1.,0.,0.));
#4882=DIRECTION('',(1.,0.,0.));
#4883=DIRECTION('',(0.,0.,1.));
#4884=DIRECTION('center_axis',(0.,0.,1.));
#4885=DIRECTION('ref_axis',(0.,1.,0.));
#4886=DIRECTION('center_axis',(0.,0.,-1.));
#4887=DIRECTION('ref_axis',(0.,1.,0.));
#4888=DIRECTION('center_axis',(0.,0.,-1.));
#4889=DIRECTION('ref_axis',(0.,1.,0.));
#4890=DIRECTION('center_axis',(-1.,-3.51417407375166E-16,0.));
#4891=DIRECTION('ref_axis',(3.51417407375166E-16,-1.,0.));
#4892=DIRECTION('',(0.,-1.,0.));
#4893=DIRECTION('',(0.,0.,1.));
#4894=DIRECTION('',(3.51417407375166E-16,-1.,0.));
#4895=DIRECTION('center_axis',(0.,0.,1.));
#4896=DIRECTION('ref_axis',(3.55271367880049E-15,-1.,0.));
#4897=DIRECTION('center_axis',(0.,0.,1.));
#4898=DIRECTION('ref_axis',(3.55271367880049E-15,-1.,0.));
#4899=DIRECTION('center_axis',(0.,0.,1.));
#4900=DIRECTION('ref_axis',(3.55271367880049E-15,-1.,0.));
#4901=DIRECTION('',(0.,0.,1.));
#4902=DIRECTION('center_axis',(-2.36032074788338E-16,-1.,0.));
#4903=DIRECTION('ref_axis',(1.,-2.36032074788338E-16,0.));
#4904=DIRECTION('',(-1.,2.36032074788338E-16,0.));
#4905=DIRECTION('',(1.,-2.36032074788338E-16,0.));
#4906=DIRECTION('',(0.,0.,1.));
#4907=DIRECTION('center_axis',(0.,0.,1.));
#4908=DIRECTION('ref_axis',(-1.,0.,0.));
#4909=DIRECTION('center_axis',(0.,0.,1.));
#4910=DIRECTION('ref_axis',(-1.,0.,0.));
#4911=DIRECTION('center_axis',(0.,0.,1.));
#4912=DIRECTION('ref_axis',(-1.,0.,0.));
#4913=DIRECTION('center_axis',(0.,0.,1.));
#4914=DIRECTION('ref_axis',(1.,0.,0.));
#4915=DIRECTION('center_axis',(0.,0.,1.));
#4916=DIRECTION('ref_axis',(1.,0.,0.));
#4917=DIRECTION('axis',(0.,0.,1.));
#4918=DIRECTION('refdir',(1.,0.,0.));
#4919=DIRECTION('center_axis',(0.,1.,0.));
#4920=DIRECTION('ref_axis',(0.,0.,-1.));
#4921=DIRECTION('center_axis',(0.,1.,0.));
#4922=DIRECTION('ref_axis',(1.,0.,0.));
#4923=DIRECTION('center_axis',(1.,0.,0.));
#4924=DIRECTION('ref_axis',(0.,0.,1.));
#4925=DIRECTION('center_axis',(0.,-1.,0.));
#4926=DIRECTION('ref_axis',(0.,0.,1.));
#4927=DIRECTION('center_axis',(0.,-1.,0.));
#4928=DIRECTION('ref_axis',(1.,0.,0.));
#4929=DIRECTION('center_axis',(0.,1.,0.));
#4930=DIRECTION('ref_axis',(0.,0.,-1.));
#4931=DIRECTION('center_axis',(0.,1.,0.));
#4932=DIRECTION('ref_axis',(1.,0.,0.));
#4933=DIRECTION('center_axis',(1.,0.,0.));
#4934=DIRECTION('ref_axis',(0.,0.,1.));
#4935=DIRECTION('center_axis',(0.,-1.,0.));
#4936=DIRECTION('ref_axis',(0.,0.,1.));
#4937=DIRECTION('center_axis',(0.,-1.,0.));
#4938=DIRECTION('ref_axis',(1.,0.,0.));
#4939=DIRECTION('center_axis',(-1.,0.,0.));
#4940=DIRECTION('ref_axis',(0.,-0.707106781186547,-0.707106781186548));
#4941=DIRECTION('center_axis',(-0.924850298995146,0.,0.380331335086382));
#4942=DIRECTION('ref_axis',(-0.380331335086382,3.4226336542529E-16,-0.924850298995146));
#4943=DIRECTION('',(1.,0.,0.));
#4944=DIRECTION('center_axis',(0.924850298995146,0.,0.380331335086382));
#4945=DIRECTION('ref_axis',(0.380331335086382,0.,-0.924850298995146));
#4946=DIRECTION('',(-1.,0.,0.));
#4947=DIRECTION('center_axis',(0.,0.,-1.));
#4948=DIRECTION('ref_axis',(1.,0.,0.));
#4949=DIRECTION('',(0.,-1.,0.));
#4950=DIRECTION('center_axis',(0.,0.,-1.));
#4951=DIRECTION('ref_axis',(3.55271367880049E-15,1.,0.));
#4952=DIRECTION('',(1.,2.36032074788338E-16,0.));
#4953=DIRECTION('center_axis',(0.,0.,-1.));
#4954=DIRECTION('ref_axis',(-1.,0.,0.));
#4955=DIRECTION('',(3.51417407375166E-16,1.,0.));
#4956=DIRECTION('center_axis',(0.,0.,1.));
#4957=DIRECTION('ref_axis',(0.,-1.,0.));
#4958=DIRECTION('',(-1.,0.,0.));
#4959=DIRECTION('center_axis',(0.,0.,1.));
#4960=DIRECTION('ref_axis',(0.,1.,0.));
#4961=DIRECTION('',(1.,0.,0.));
#4962=DIRECTION('center_axis',(0.,0.,1.));
#4963=DIRECTION('ref_axis',(0.,-1.,0.));
#4964=DIRECTION('',(-1.,0.,0.));
#4965=DIRECTION('center_axis',(0.,0.,1.));
#4966=DIRECTION('ref_axis',(0.,1.,0.));
#4967=DIRECTION('',(1.,0.,0.));
#4968=DIRECTION('center_axis',(0.,-1.,0.));
#4969=DIRECTION('ref_axis',(-0.707106781186548,0.,0.707106781186548));
#4970=DIRECTION('center_axis',(0.,1.,0.));
#4971=DIRECTION('ref_axis',(-0.707106781186548,0.,0.707106781186548));
#4972=DIRECTION('',(0.,1.,0.));
#4973=DIRECTION('center_axis',(0.,-1.,0.));
#4974=DIRECTION('ref_axis',(-0.707106781186548,0.,0.707106781186548));
#4975=DIRECTION('',(0.,-1.,0.));
#4976=DIRECTION('center_axis',(0.,0.,-1.));
#4977=DIRECTION('ref_axis',(1.,0.,0.));
#4978=DIRECTION('',(-1.,0.,0.));
#4979=DIRECTION('',(0.,1.,0.));
#4980=DIRECTION('',(1.,0.,0.));
#4981=DIRECTION('center_axis',(0.,-1.,0.));
#4982=DIRECTION('ref_axis',(1.,0.,0.));
#4983=DIRECTION('',(-0.380331335086382,0.,-0.924850298995146));
#4984=DIRECTION('center_axis',(0.,1.,0.));
#4985=DIRECTION('ref_axis',(-0.556627642555424,0.,0.830762100449455));
#4986=DIRECTION('',(1.,0.,0.));
#4987=DIRECTION('center_axis',(0.,1.,0.));
#4988=DIRECTION('ref_axis',(0.707106781186548,0.,0.707106781186548));
#4989=DIRECTION('',(0.,0.,1.));
#4990=DIRECTION('center_axis',(0.,1.,0.));
#4991=DIRECTION('ref_axis',(-1.,0.,-1.85962356624686E-14));
#4992=DIRECTION('center_axis',(0.,1.,0.));
#4993=DIRECTION('ref_axis',(-0.965748659616478,0.,-0.259479337229339));
#4994=DIRECTION('center_axis',(0.,1.,0.));
#4995=DIRECTION('ref_axis',(0.965748659616483,0.,-0.259479337229319));
#4996=DIRECTION('',(0.,0.,-1.));
#4997=DIRECTION('center_axis',(0.,1.,0.));
#4998=DIRECTION('ref_axis',(0.556627642555425,0.,0.830762100449455));
#4999=DIRECTION('',(-0.380331335086382,0.,0.924850298995146));
#5000=DIRECTION('center_axis',(0.,1.,0.));
#5001=DIRECTION('ref_axis',(0.707106781186548,0.,0.707106781186548));
#5002=DIRECTION('center_axis',(0.,-1.,0.));
#5003=DIRECTION('ref_axis',(0.707106781186548,0.,0.707106781186548));
#5004=DIRECTION('',(0.,-1.,0.));
#5005=DIRECTION('',(0.,1.,0.));
#5006=DIRECTION('center_axis',(1.,0.,0.));
#5007=DIRECTION('ref_axis',(0.,0.,1.));
#5008=DIRECTION('',(0.,0.,-1.));
#5009=DIRECTION('',(0.,-1.,0.));
#5010=DIRECTION('center_axis',(0.,1.,0.));
#5011=DIRECTION('ref_axis',(0.556627642555425,0.,0.830762100449455));
#5012=DIRECTION('center_axis',(0.,-1.,0.));
#5013=DIRECTION('ref_axis',(0.556627642555425,0.,0.830762100449455));
#5014=DIRECTION('',(0.,-1.,0.));
#5015=DIRECTION('center_axis',(0.924850298995146,0.,0.380331335086382));
#5016=DIRECTION('ref_axis',(-0.380331335086382,0.,0.924850298995145));
#5017=DIRECTION('',(0.380331335086382,0.,-0.924850298995146));
#5018=DIRECTION('',(0.,-1.,0.));
#5019=DIRECTION('center_axis',(0.,-1.,0.));
#5020=DIRECTION('ref_axis',(-0.556627642555424,0.,0.830762100449455));
#5021=DIRECTION('',(0.,1.,0.));
#5022=DIRECTION('center_axis',(0.,-1.,0.));
#5023=DIRECTION('ref_axis',(-0.556627642555424,0.,0.830762100449455));
#5024=DIRECTION('',(0.,-1.,0.));
#5025=DIRECTION('center_axis',(-0.924850298995146,0.,0.380331335086382));
#5026=DIRECTION('ref_axis',(-0.380331335086382,0.,-0.924850298995145));
#5027=DIRECTION('',(-3.51417407375166E-16,-1.,-8.54540408060787E-16));
#5028=DIRECTION('',(0.380331335086382,0.,0.924850298995146));
#5029=DIRECTION('center_axis',(0.,1.,0.));
#5030=DIRECTION('ref_axis',(0.965748659616483,0.,-0.259479337229319));
#5031=DIRECTION('center_axis',(0.,-1.,0.));
#5032=DIRECTION('ref_axis',(0.965748659616483,0.,-0.259479337229319));
#5033=DIRECTION('',(0.,-1.,0.));
#5034=DIRECTION('',(0.,-1.,0.));
#5035=DIRECTION('center_axis',(-1.,0.,0.));
#5036=DIRECTION('ref_axis',(0.,0.,-1.));
#5037=DIRECTION('',(0.,0.,1.));
#5038=DIRECTION('center_axis',(0.,1.,0.));
#5039=DIRECTION('ref_axis',(-1.,0.,-1.85962356624686E-14));
#5040=DIRECTION('center_axis',(0.,-1.,0.));
#5041=DIRECTION('ref_axis',(-1.,0.,-1.85962356624686E-14));
#5042=DIRECTION('',(0.,-1.,0.));
#5043=DIRECTION('center_axis',(0.,1.,0.));
#5044=DIRECTION('ref_axis',(-0.965748659616478,0.,-0.259479337229339));
#5045=DIRECTION('center_axis',(0.,-1.,0.));
#5046=DIRECTION('ref_axis',(-0.965748659616478,0.,-0.259479337229339));
#5047=DIRECTION('center_axis',(-1.,0.,0.));
#5048=DIRECTION('ref_axis',(0.,-1.,0.));
#5049=DIRECTION('',(0.,0.,1.));
#5050=DIRECTION('',(0.,1.,0.));
#5051=DIRECTION('',(0.,0.,1.));
#5052=DIRECTION('center_axis',(0.,1.,0.));
#5053=DIRECTION('ref_axis',(-1.,0.,0.));
#5054=DIRECTION('',(-1.,0.,0.));
#5055=DIRECTION('',(0.,0.,1.));
#5056=DIRECTION('',(-1.,0.,0.));
#5057=DIRECTION('center_axis',(0.,0.,-1.));
#5058=DIRECTION('ref_axis',(1.,0.,0.));
#5059=DIRECTION('center_axis',(0.,1.,0.));
#5060=DIRECTION('ref_axis',(-1.,0.,0.));
#5061=DIRECTION('',(-1.,0.,0.));
#5062=DIRECTION('',(0.,0.,1.));
#5063=DIRECTION('',(0.,0.,1.));
#5064=DIRECTION('center_axis',(0.,0.,-1.));
#5065=DIRECTION('ref_axis',(0.,1.,0.));
#5066=DIRECTION('center_axis',(0.,0.,1.));
#5067=DIRECTION('ref_axis',(0.,1.,0.));
#5068=DIRECTION('',(0.,0.,1.));
#5069=DIRECTION('center_axis',(0.,-1.,0.));
#5070=DIRECTION('ref_axis',(1.,0.,0.));
#5071=DIRECTION('',(1.,0.,0.));
#5072=DIRECTION('',(0.,0.,1.));
#5073=DIRECTION('center_axis',(0.,0.,-1.));
#5074=DIRECTION('ref_axis',(0.,-1.,0.));
#5075=DIRECTION('center_axis',(0.,0.,1.));
#5076=DIRECTION('ref_axis',(0.,-1.,0.));
#5077=DIRECTION('center_axis',(0.,1.,0.));
#5078=DIRECTION('ref_axis',(-1.,0.,0.));
#5079=DIRECTION('',(-1.,0.,0.));
#5080=DIRECTION('',(0.,0.,1.));
#5081=DIRECTION('',(0.,0.,1.));
#5082=DIRECTION('center_axis',(0.,0.,-1.));
#5083=DIRECTION('ref_axis',(0.,1.,0.));
#5084=DIRECTION('center_axis',(0.,0.,1.));
#5085=DIRECTION('ref_axis',(0.,1.,0.));
#5086=DIRECTION('',(0.,0.,1.));
#5087=DIRECTION('center_axis',(0.,-1.,0.));
#5088=DIRECTION('ref_axis',(1.,0.,0.));
#5089=DIRECTION('',(1.,0.,0.));
#5090=DIRECTION('',(0.,0.,1.));
#5091=DIRECTION('center_axis',(0.,0.,-1.));
#5092=DIRECTION('ref_axis',(0.,-1.,0.));
#5093=DIRECTION('center_axis',(0.,0.,1.));
#5094=DIRECTION('ref_axis',(0.,-1.,0.));
#5095=DIRECTION('center_axis',(1.,-3.51417407375166E-16,0.));
#5096=DIRECTION('ref_axis',(3.51417407375166E-16,1.,0.));
#5097=DIRECTION('',(0.,0.,1.));
#5098=DIRECTION('',(0.,1.,0.));
#5099=DIRECTION('center_axis',(0.,0.,-1.));
#5100=DIRECTION('ref_axis',(3.55271367880049E-15,1.,0.));
#5101=DIRECTION('center_axis',(0.,0.,-1.));
#5102=DIRECTION('ref_axis',(3.55271367880049E-15,1.,0.));
#5103=DIRECTION('',(0.,0.,1.));
#5104=DIRECTION('center_axis',(2.36032074788338E-16,-1.,0.));
#5105=DIRECTION('ref_axis',(1.,2.36032074788338E-16,0.));
#5106=DIRECTION('',(-1.,-2.36032074788338E-16,0.));
#5107=DIRECTION('',(0.,0.,1.));
#5108=DIRECTION('center_axis',(0.,0.,-1.));
#5109=DIRECTION('ref_axis',(-1.,0.,0.));
#5110=DIRECTION('center_axis',(0.,0.,-1.));
#5111=DIRECTION('ref_axis',(-1.,0.,0.));
#5112=DIRECTION('center_axis',(0.,0.,-1.));
#5113=DIRECTION('ref_axis',(1.,0.,0.));
#5114=DIRECTION('axis',(0.,0.,1.));
#5115=DIRECTION('refdir',(1.,0.,0.));
#5116=DIRECTION('center_axis',(0.,0.,-1.));
#5117=DIRECTION('ref_axis',(-1.,0.,0.));
#5118=DIRECTION('center_axis',(0.,0.,-1.));
#5119=DIRECTION('ref_axis',(-1.,0.,0.));
#5120=DIRECTION('',(0.,0.,-1.));
#5121=DIRECTION('center_axis',(0.,0.,1.));
#5122=DIRECTION('ref_axis',(-1.,0.,0.));
#5123=DIRECTION('center_axis',(0.866025403784439,-0.5,0.));
#5124=DIRECTION('ref_axis',(-0.5,-0.866025403784439,0.));
#5125=DIRECTION('',(0.5,0.866025403784439,0.));
#5126=DIRECTION('',(0.,0.,-1.));
#5127=DIRECTION('',(-0.5,-0.866025403784439,0.));
#5128=DIRECTION('',(0.,0.,-1.));
#5129=DIRECTION('center_axis',(0.866025403784439,0.5,0.));
#5130=DIRECTION('ref_axis',(0.5,-0.866025403784439,0.));
#5131=DIRECTION('',(-0.5,0.866025403784439,0.));
#5132=DIRECTION('',(0.5,-0.866025403784439,0.));
#5133=DIRECTION('',(0.,0.,-1.));
#5134=DIRECTION('center_axis',(4.80740671595891E-16,1.,0.));
#5135=DIRECTION('ref_axis',(1.,-4.80740671595891E-16,0.));
#5136=DIRECTION('',(-1.,4.80740671595891E-16,0.));
#5137=DIRECTION('',(1.,-4.80740671595891E-16,0.));
#5138=DIRECTION('',(0.,0.,-1.));
#5139=DIRECTION('center_axis',(-0.866025403784438,0.500000000000001,0.));
#5140=DIRECTION('ref_axis',(0.500000000000001,0.866025403784438,0.));
#5141=DIRECTION('',(-0.500000000000001,-0.866025403784438,0.));
#5142=DIRECTION('',(0.500000000000001,0.866025403784438,0.));
#5143=DIRECTION('',(0.,0.,-1.));
#5144=DIRECTION('center_axis',(-0.866025403784439,-0.499999999999999,0.));
#5145=DIRECTION('ref_axis',(-0.499999999999999,0.866025403784439,0.));
#5146=DIRECTION('',(0.499999999999999,-0.866025403784439,0.));
#5147=DIRECTION('',(-0.499999999999999,0.866025403784439,0.));
#5148=DIRECTION('',(0.,0.,-1.));
#5149=DIRECTION('center_axis',(-1.20185167898973E-16,-1.,0.));
#5150=DIRECTION('ref_axis',(-1.,1.20185167898973E-16,0.));
#5151=DIRECTION('',(1.,-1.20185167898973E-16,0.));
#5152=DIRECTION('',(-1.,1.20185167898973E-16,0.));
#5153=DIRECTION('center_axis',(0.,0.,1.));
#5154=DIRECTION('ref_axis',(-1.,0.,0.));
#5155=DIRECTION('center_axis',(0.,0.,1.));
#5156=DIRECTION('ref_axis',(-1.,0.,0.));
#5157=DIRECTION('axis',(0.,0.,1.));
#5158=DIRECTION('refdir',(1.,0.,0.));
#5159=DIRECTION('center_axis',(0.,0.,1.));
#5160=DIRECTION('ref_axis',(-1.,-4.17628703648668E-14,0.));
#5161=DIRECTION('',(0.,0.,-1.));
#5162=DIRECTION('center_axis',(0.,0.,-1.));
#5163=DIRECTION('ref_axis',(-1.,-4.17628703648668E-14,0.));
#5164=DIRECTION('center_axis',(0.,0.,1.));
#5165=DIRECTION('ref_axis',(-1.,-4.17628703648668E-14,0.));
#5166=DIRECTION('',(0.,0.,-1.));
#5167=DIRECTION('center_axis',(0.,0.,1.));
#5168=DIRECTION('ref_axis',(-1.,-4.17628703648668E-14,0.));
#5169=DIRECTION('',(0.,0.,-1.));
#5170=DIRECTION('center_axis',(0.,0.,1.));
#5171=DIRECTION('ref_axis',(-1.,-4.17628703648668E-14,0.));
#5172=DIRECTION('',(0.,0.,-1.));
#5173=DIRECTION('center_axis',(0.,0.,1.));
#5174=DIRECTION('ref_axis',(-1.,-4.17628703648668E-14,0.));
#5175=DIRECTION('',(0.,0.,-1.));
#5176=DIRECTION('center_axis',(0.,0.,1.));
#5177=DIRECTION('ref_axis',(-1.,-4.17628703648668E-14,0.));
#5178=DIRECTION('',(0.,0.,-1.));
#5179=DIRECTION('center_axis',(0.,0.,1.));
#5180=DIRECTION('ref_axis',(-1.,-4.17628703648668E-14,0.));
#5181=DIRECTION('',(0.,0.,-1.));
#5182=DIRECTION('center_axis',(0.,0.,1.));
#5183=DIRECTION('ref_axis',(-1.,-4.17628703648668E-14,0.));
#5184=DIRECTION('',(0.,0.,-1.));
#5185=DIRECTION('center_axis',(0.,0.,1.));
#5186=DIRECTION('ref_axis',(-1.,-4.17628703648668E-14,0.));
#5187=DIRECTION('',(0.,0.,-1.));
#5188=DIRECTION('center_axis',(0.,0.,1.));
#5189=DIRECTION('ref_axis',(-1.,-4.17628703648668E-14,0.));
#5190=DIRECTION('',(0.,0.,-1.));
#5191=DIRECTION('center_axis',(0.,0.,1.));
#5192=DIRECTION('ref_axis',(-1.,-4.17628703648668E-14,0.));
#5193=DIRECTION('',(0.,0.,-1.));
#5194=DIRECTION('center_axis',(0.,0.,1.));
#5195=DIRECTION('ref_axis',(-1.,-4.17628703648668E-14,0.));
#5196=DIRECTION('',(0.,0.,-1.));
#5197=DIRECTION('center_axis',(0.,0.,1.));
#5198=DIRECTION('ref_axis',(-1.,-4.17628703648668E-14,0.));
#5199=DIRECTION('',(0.,0.,-1.));
#5200=DIRECTION('center_axis',(0.,0.,1.));
#5201=DIRECTION('ref_axis',(-1.,-4.17628703648668E-14,0.));
#5202=DIRECTION('',(0.,0.,-1.));
#5203=DIRECTION('center_axis',(0.,0.,1.));
#5204=DIRECTION('ref_axis',(-1.,-4.17628703648668E-14,0.));
#5205=DIRECTION('',(0.,0.,-1.));
#5206=DIRECTION('center_axis',(0.,0.,1.));
#5207=DIRECTION('ref_axis',(-1.,-4.17628703648668E-14,0.));
#5208=DIRECTION('',(0.,0.,-1.));
#5209=DIRECTION('center_axis',(0.,0.,1.));
#5210=DIRECTION('ref_axis',(-1.,-4.17628703648668E-14,0.));
#5211=DIRECTION('',(0.,0.,-1.));
#5212=DIRECTION('center_axis',(0.,0.,1.));
#5213=DIRECTION('ref_axis',(-1.,-4.17628703648668E-14,0.));
#5214=DIRECTION('',(0.,0.,-1.));
#5215=DIRECTION('center_axis',(0.,0.,1.));
#5216=DIRECTION('ref_axis',(-1.,-4.17628703648668E-14,0.));
#5217=DIRECTION('',(0.,0.,-1.));
#5218=DIRECTION('center_axis',(0.,0.,1.));
#5219=DIRECTION('ref_axis',(-1.,-4.17628703648668E-14,0.));
#5220=DIRECTION('',(0.,0.,-1.));
#5221=DIRECTION('center_axis',(0.,0.,1.));
#5222=DIRECTION('ref_axis',(-1.,-4.17628703648668E-14,0.));
#5223=DIRECTION('',(0.,0.,-1.));
#5224=DIRECTION('center_axis',(0.,0.,1.));
#5225=DIRECTION('ref_axis',(-1.,-4.17628703648668E-14,0.));
#5226=DIRECTION('',(0.,0.,-1.));
#5227=DIRECTION('center_axis',(0.,0.,1.));
#5228=DIRECTION('ref_axis',(-1.,0.,0.));
#5229=DIRECTION('center_axis',(0.,0.,-1.));
#5230=DIRECTION('ref_axis',(-1.,0.,0.));
#5231=DIRECTION('center_axis',(0.,0.,-1.));
#5232=DIRECTION('ref_axis',(-1.,0.,0.));
#5233=DIRECTION('center_axis',(0.,0.,1.));
#5234=DIRECTION('ref_axis',(-1.,-4.17628703648668E-14,0.));
#5235=DIRECTION('center_axis',(0.,0.,1.));
#5236=DIRECTION('ref_axis',(-1.,-4.17628703648668E-14,0.));
#5237=DIRECTION('center_axis',(0.,0.,1.));
#5238=DIRECTION('ref_axis',(-1.,0.,0.));
#5239=DIRECTION('center_axis',(0.,0.,1.));
#5240=DIRECTION('ref_axis',(1.,0.,0.));
#5241=DIRECTION('center_axis',(0.,0.,-1.));
#5242=DIRECTION('ref_axis',(1.,0.,0.));
#5243=DIRECTION('center_axis',(0.,0.,-1.));
#5244=DIRECTION('ref_axis',(-1.,0.,0.));
#5245=DIRECTION('center_axis',(0.,0.,-1.));
#5246=DIRECTION('ref_axis',(1.,0.,0.));
#5247=DIRECTION('',(-0.966586729160533,1.18372734396476E-16,0.256339803797111));
#5248=DIRECTION('center_axis',(0.,0.,1.));
#5249=DIRECTION('ref_axis',(-1.,0.,0.));
#5250=DIRECTION('',(-0.237251396871265,-2.90549163771633E-17,-0.971448287189099));
#5251=DIRECTION('center_axis',(0.,0.,-1.));
#5252=DIRECTION('ref_axis',(1.,0.,0.));
#5253=DIRECTION('center_axis',(0.,0.,-1.));
#5254=DIRECTION('ref_axis',(-1.,0.,0.));
#5255=DIRECTION('axis',(0.,0.,1.));
#5256=DIRECTION('refdir',(1.,0.,0.));
#5257=DIRECTION('center_axis',(0.,0.,-1.));
#5258=DIRECTION('ref_axis',(-1.,0.,0.));
#5259=DIRECTION('center_axis',(0.,0.,-1.));
#5260=DIRECTION('ref_axis',(-1.,0.,0.));
#5261=DIRECTION('',(0.,0.,-1.));
#5262=DIRECTION('center_axis',(0.,0.,1.));
#5263=DIRECTION('ref_axis',(-1.,0.,0.));
#5264=DIRECTION('center_axis',(0.866025403784439,-0.5,0.));
#5265=DIRECTION('ref_axis',(-0.5,-0.866025403784439,0.));
#5266=DIRECTION('',(0.5,0.866025403784439,0.));
#5267=DIRECTION('',(0.,0.,-1.));
#5268=DIRECTION('',(-0.5,-0.866025403784439,0.));
#5269=DIRECTION('',(0.,0.,-1.));
#5270=DIRECTION('center_axis',(0.866025403784439,0.5,0.));
#5271=DIRECTION('ref_axis',(0.5,-0.866025403784439,0.));
#5272=DIRECTION('',(-0.5,0.866025403784439,0.));
#5273=DIRECTION('',(0.5,-0.866025403784439,0.));
#5274=DIRECTION('',(0.,0.,-1.));
#5275=DIRECTION('center_axis',(4.80740671595891E-16,1.,0.));
#5276=DIRECTION('ref_axis',(1.,-4.80740671595891E-16,0.));
#5277=DIRECTION('',(-1.,4.80740671595891E-16,0.));
#5278=DIRECTION('',(1.,-4.80740671595891E-16,0.));
#5279=DIRECTION('',(0.,0.,-1.));
#5280=DIRECTION('center_axis',(-0.866025403784438,0.500000000000001,0.));
#5281=DIRECTION('ref_axis',(0.500000000000001,0.866025403784438,0.));
#5282=DIRECTION('',(-0.500000000000001,-0.866025403784438,0.));
#5283=DIRECTION('',(0.500000000000001,0.866025403784438,0.));
#5284=DIRECTION('',(0.,0.,-1.));
#5285=DIRECTION('center_axis',(-0.866025403784439,-0.499999999999999,0.));
#5286=DIRECTION('ref_axis',(-0.499999999999999,0.866025403784439,0.));
#5287=DIRECTION('',(0.499999999999999,-0.866025403784439,0.));
#5288=DIRECTION('',(-0.499999999999999,0.866025403784439,0.));
#5289=DIRECTION('',(0.,0.,-1.));
#5290=DIRECTION('center_axis',(-1.20185167898973E-16,-1.,0.));
#5291=DIRECTION('ref_axis',(-1.,1.20185167898973E-16,0.));
#5292=DIRECTION('',(1.,-1.20185167898973E-16,0.));
#5293=DIRECTION('',(-1.,1.20185167898973E-16,0.));
#5294=DIRECTION('center_axis',(0.,0.,1.));
#5295=DIRECTION('ref_axis',(-1.,0.,0.));
#5296=DIRECTION('center_axis',(0.,0.,1.));
#5297=DIRECTION('ref_axis',(-1.,0.,0.));
#5298=DIRECTION('axis',(0.,0.,1.));
#5299=DIRECTION('refdir',(1.,0.,0.));
#5300=DIRECTION('center_axis',(0.,1.,0.));
#5301=DIRECTION('ref_axis',(0.148020831985877,0.,-0.988984243200168));
#5302=DIRECTION('center_axis',(0.,1.,0.));
#5303=DIRECTION('ref_axis',(0.148020831985877,0.,-0.988984243200168));
#5304=DIRECTION('center_axis',(0.999483033337749,0.,-0.0321506775973911));
#5305=DIRECTION('ref_axis',(0.,1.,0.));
#5306=DIRECTION('center_axis',(0.,-1.,0.));
#5307=DIRECTION('ref_axis',(0.148020831985877,0.,-0.988984243200168));
#5308=DIRECTION('center_axis',(0.,1.,0.));
#5309=DIRECTION('ref_axis',(0.,0.,1.));
#5310=DIRECTION('center_axis',(0.,-1.,0.));
#5311=DIRECTION('ref_axis',(-0.143870612043421,0.,-0.989596507163526));
#5312=DIRECTION('center_axis',(0.,1.,0.));
#5313=DIRECTION('ref_axis',(-0.143870612043421,0.,-0.989596507163526));
#5314=DIRECTION('center_axis',(0.,-1.,0.));
#5315=DIRECTION('ref_axis',(-0.0321506775973877,0.,-0.999483033337749));
#5316=DIRECTION('',(0.,-1.,0.));
#5317=DIRECTION('center_axis',(0.,1.,0.));
#5318=DIRECTION('ref_axis',(0.148020831985877,0.,-0.988984243200168));
#5319=DIRECTION('',(0.,-1.,0.));
#5320=DIRECTION('center_axis',(0.,-1.,0.));
#5321=DIRECTION('ref_axis',(-0.253780785521889,0.,-0.967261760279963));
#5322=DIRECTION('',(0.,-1.,0.));
#5323=DIRECTION('center_axis',(0.,1.,0.));
#5324=DIRECTION('ref_axis',(-0.143870612043421,0.,-0.989596507163526));
#5325=DIRECTION('center_axis',(0.,-1.,0.));
#5326=DIRECTION('ref_axis',(-0.125259595502011,0.,-0.992124001188698));
#5327=DIRECTION('center_axis',(0.,1.,0.));
#5328=DIRECTION('ref_axis',(-0.125259595502011,0.,-0.992124001188698));
#5329=DIRECTION('',(0.,1.,0.));
#5330=DIRECTION('',(0.,1.,0.));
#5331=DIRECTION('',(0.,-1.,0.));
#5332=DIRECTION('center_axis',(0.,1.,0.));
#5333=DIRECTION('ref_axis',(-0.125259595502011,0.,-0.992124001188698));
#5334=DIRECTION('center_axis',(0.,1.,0.));
#5335=DIRECTION('ref_axis',(0.148020831985877,0.,-0.988984243200168));
#5336=DIRECTION('center_axis',(0.999483033337749,0.,-0.0321506775973911));
#5337=DIRECTION('ref_axis',(0.0321506775973911,0.,0.999483033337749));
#5338=DIRECTION('center_axis',(0.,-1.,0.));
#5339=DIRECTION('ref_axis',(0.148020831985877,0.,-0.988984243200168));
#5340=DIRECTION('center_axis',(0.,1.,0.));
#5341=DIRECTION('ref_axis',(0.,0.,1.));
#5342=DIRECTION('center_axis',(0.,-1.,0.));
#5343=DIRECTION('ref_axis',(-0.143870612043421,0.,-0.989596507163526));
#5344=DIRECTION('center_axis',(0.,-1.,0.));
#5345=DIRECTION('ref_axis',(-1.,0.,0.));
#5346=DIRECTION('',(-0.992124001188699,0.,0.12525959550201));
#5347=DIRECTION('center_axis',(0.,-1.,0.));
#5348=DIRECTION('ref_axis',(-1.,0.,0.));
#5349=DIRECTION('center_axis',(0.,1.,0.));
#5350=DIRECTION('ref_axis',(0.702611585857253,0.,0.711573579764704));
#5351=DIRECTION('center_axis',(0.,-1.,0.));
#5352=DIRECTION('ref_axis',(-1.,0.,0.));
#5353=DIRECTION('',(0.,0.,1.));
#5354=DIRECTION('center_axis',(0.,1.,0.));
#5355=DIRECTION('ref_axis',(0.,0.,-1.));
#5356=DIRECTION('center_axis',(0.,1.,0.));
#5357=DIRECTION('ref_axis',(0.,0.,-1.));
#5358=DIRECTION('center_axis',(0.,-1.,0.));
#5359=DIRECTION('ref_axis',(1.,0.,0.));
#5360=DIRECTION('center_axis',(0.,1.,0.));
#5361=DIRECTION('ref_axis',(-1.,0.,0.));
#5362=DIRECTION('center_axis',(0.,-1.,0.));
#5363=DIRECTION('ref_axis',(-1.,0.,0.));
#5364=DIRECTION('center_axis',(0.,1.,0.));
#5365=DIRECTION('ref_axis',(-1.,0.,0.));
#5366=DIRECTION('center_axis',(0.,0.,1.));
#5367=DIRECTION('ref_axis',(1.,0.,0.));
#5368=DIRECTION('center_axis',(0.,-1.,0.));
#5369=DIRECTION('ref_axis',(1.,0.,0.));
#5370=DIRECTION('center_axis',(0.,-1.,0.));
#5371=DIRECTION('ref_axis',(1.,0.,0.));
#5372=DIRECTION('center_axis',(0.,1.,0.));
#5373=DIRECTION('ref_axis',(-1.,0.,0.));
#5374=DIRECTION('center_axis',(0.,-1.,0.));
#5375=DIRECTION('ref_axis',(-1.,0.,0.));
#5376=DIRECTION('center_axis',(0.,1.,0.));
#5377=DIRECTION('ref_axis',(-1.,0.,0.));
#5378=DIRECTION('center_axis',(0.,0.,1.));
#5379=DIRECTION('ref_axis',(1.,0.,0.));
#5380=DIRECTION('center_axis',(0.,-1.,0.));
#5381=DIRECTION('ref_axis',(1.,0.,0.));
#5382=DIRECTION('center_axis',(0.,-1.,0.));
#5383=DIRECTION('ref_axis',(1.,0.,0.));
#5384=DIRECTION('center_axis',(0.,1.,0.));
#5385=DIRECTION('ref_axis',(-1.,0.,0.));
#5386=DIRECTION('center_axis',(0.,1.,0.));
#5387=DIRECTION('ref_axis',(-1.,0.,0.));
#5388=DIRECTION('center_axis',(0.,1.,0.));
#5389=DIRECTION('ref_axis',(-1.,0.,0.));
#5390=DIRECTION('center_axis',(0.,0.,-1.));
#5391=DIRECTION('ref_axis',(1.,0.,0.));
#5392=DIRECTION('center_axis',(0.,-1.,0.));
#5393=DIRECTION('ref_axis',(0.,0.,1.));
#5394=DIRECTION('center_axis',(0.,-1.,0.));
#5395=DIRECTION('ref_axis',(1.,0.,0.));
#5396=DIRECTION('center_axis',(0.,-1.,0.));
#5397=DIRECTION('ref_axis',(1.,0.,0.));
#5398=DIRECTION('center_axis',(0.,1.,0.));
#5399=DIRECTION('ref_axis',(-1.,0.,0.));
#5400=DIRECTION('center_axis',(0.,1.,0.));
#5401=DIRECTION('ref_axis',(-1.,0.,0.));
#5402=DIRECTION('center_axis',(0.,1.,0.));
#5403=DIRECTION('ref_axis',(-1.,0.,0.));
#5404=DIRECTION('center_axis',(0.,0.,-1.));
#5405=DIRECTION('ref_axis',(1.,0.,0.));
#5406=DIRECTION('center_axis',(0.,-1.,0.));
#5407=DIRECTION('ref_axis',(0.,0.,1.));
#5408=DIRECTION('center_axis',(0.,-1.,0.));
#5409=DIRECTION('ref_axis',(1.,0.,0.));
#5410=DIRECTION('center_axis',(0.,-1.,0.));
#5411=DIRECTION('ref_axis',(-1.,0.,0.));
#5412=DIRECTION('',(0.,-1.,0.));
#5413=DIRECTION('center_axis',(0.,1.,0.));
#5414=DIRECTION('ref_axis',(-1.,0.,0.));
#5415=DIRECTION('center_axis',(0.,-1.,0.));
#5416=DIRECTION('ref_axis',(-1.,0.,0.));
#5417=DIRECTION('',(0.,-1.,0.));
#5418=DIRECTION('center_axis',(0.,1.,0.));
#5419=DIRECTION('ref_axis',(-1.,0.,0.));
#5420=DIRECTION('center_axis',(-0.12525959550201,0.,-0.992124001188699));
#5421=DIRECTION('ref_axis',(-0.992124001188699,0.,0.12525959550201));
#5422=DIRECTION('',(0.992124001188699,0.,-0.12525959550201));
#5423=DIRECTION('',(-0.992124001188699,0.,0.12525959550201));
#5424=DIRECTION('',(0.,1.,0.));
#5425=DIRECTION('',(0.,1.,0.));
#5426=DIRECTION('',(0.,1.,0.));
#5427=DIRECTION('center_axis',(0.,-1.,0.));
#5428=DIRECTION('ref_axis',(-1.,0.,0.));
#5429=DIRECTION('center_axis',(0.,-1.,0.));
#5430=DIRECTION('ref_axis',(-1.,0.,0.));
#5431=DIRECTION('',(0.,1.,0.));
#5432=DIRECTION('center_axis',(0.,-1.,0.));
#5433=DIRECTION('ref_axis',(-1.,0.,0.));
#5434=DIRECTION('center_axis',(0.,-1.,0.));
#5435=DIRECTION('ref_axis',(0.702611585857253,0.,0.711573579764704));
#5436=DIRECTION('center_axis',(0.,-1.,0.));
#5437=DIRECTION('ref_axis',(0.702611585857253,0.,0.711573579764704));
#5438=DIRECTION('',(0.,1.,0.));
#5439=DIRECTION('center_axis',(0.,1.,0.));
#5440=DIRECTION('ref_axis',(0.702611585857253,0.,0.711573579764704));
#5441=DIRECTION('center_axis',(0.,-1.,0.));
#5442=DIRECTION('ref_axis',(-1.,0.,0.));
#5443=DIRECTION('center_axis',(0.,-1.,0.));
#5444=DIRECTION('ref_axis',(-1.,0.,0.));
#5445=DIRECTION('center_axis',(0.,-1.,0.));
#5446=DIRECTION('ref_axis',(-1.,0.,0.));
#5447=DIRECTION('center_axis',(0.,-1.,0.));
#5448=DIRECTION('ref_axis',(-1.,0.,0.));
#5449=DIRECTION('',(0.,0.,1.));
#5450=DIRECTION('center_axis',(0.,-1.,0.));
#5451=DIRECTION('ref_axis',(-1.,0.,0.));
#5452=DIRECTION('',(0.987175716907317,0.,-0.159637413999743));
#5453=DIRECTION('',(0.,0.,-1.));
#5454=DIRECTION('center_axis',(0.,-1.,0.));
#5455=DIRECTION('ref_axis',(-0.0321506775973883,0.,-0.999483033337749));
#5456=DIRECTION('center_axis',(0.,-1.,0.));
#5457=DIRECTION('ref_axis',(-0.25378078552189,0.,-0.967261760279963));
#5458=DIRECTION('center_axis',(-0.159637413999743,0.,-0.987175716907317));
#5459=DIRECTION('ref_axis',(-0.987175716907317,0.,0.159637413999743));
#5460=DIRECTION('',(0.,1.,0.));
#5461=DIRECTION('',(0.987175716907317,0.,-0.159637413999743));
#5462=DIRECTION('center_axis',(0.,1.,0.));
#5463=DIRECTION('ref_axis',(-0.25378078552189,0.,-0.967261760279963));
#5464=DIRECTION('',(0.,1.,0.));
#5465=DIRECTION('center_axis',(0.,-1.,0.));
#5466=DIRECTION('ref_axis',(-0.25378078552189,0.,-0.967261760279963));
#5467=DIRECTION('center_axis',(0.,1.,0.));
#5468=DIRECTION('ref_axis',(-0.0321506775973883,0.,-0.999483033337749));
#5469=DIRECTION('',(0.,1.,0.));
#5470=DIRECTION('center_axis',(0.,-1.,0.));
#5471=DIRECTION('ref_axis',(-0.0321506775973883,0.,-0.999483033337749));
#5472=DIRECTION('center_axis',(0.,-1.,0.));
#5473=DIRECTION('ref_axis',(-1.,0.,0.));
#5474=DIRECTION('',(0.,0.,-1.));
#5475=DIRECTION('center_axis',(0.,-1.,0.));
#5476=DIRECTION('ref_axis',(-1.,0.,0.));
#5477=DIRECTION('center_axis',(0.,-1.,0.));
#5478=DIRECTION('ref_axis',(0.702611585857253,0.,0.711573579764704));
#5479=DIRECTION('center_axis',(0.,-1.,0.));
#5480=DIRECTION('ref_axis',(-1.,0.,0.));
#5481=DIRECTION('',(0.992124001188699,0.,-0.12525959550201));
#5482=DIRECTION('center_axis',(0.,1.,0.));
#5483=DIRECTION('ref_axis',(-1.,0.,0.));
#5484=DIRECTION('center_axis',(0.,1.,0.));
#5485=DIRECTION('ref_axis',(-1.,0.,0.));
#5486=DIRECTION('center_axis',(0.,-1.,0.));
#5487=DIRECTION('ref_axis',(-1.,0.,0.));
#5488=DIRECTION('',(0.,-1.,0.));
#5489=DIRECTION('center_axis',(0.,-1.,0.));
#5490=DIRECTION('ref_axis',(-1.,0.,0.));
#5491=DIRECTION('',(0.,-1.,0.));
#5492=DIRECTION('center_axis',(0.12525959550201,0.,0.992124001188699));
#5493=DIRECTION('ref_axis',(-0.992124001188699,0.,0.12525959550201));
#5494=DIRECTION('',(0.,-1.,0.));
#5495=DIRECTION('center_axis',(1.,0.,0.));
#5496=DIRECTION('ref_axis',(0.,0.,1.));
#5497=DIRECTION('',(0.,-1.,0.));
#5498=DIRECTION('',(0.,-1.,0.));
#5499=DIRECTION('center_axis',(0.,-1.,0.));
#5500=DIRECTION('ref_axis',(-1.,0.,0.));
#5501=DIRECTION('',(0.,-1.,0.));
#5502=DIRECTION('center_axis',(0.,-1.,0.));
#5503=DIRECTION('ref_axis',(0.702611585857253,0.,0.711573579764704));
#5504=DIRECTION('',(0.,-1.,0.));
#5505=DIRECTION('center_axis',(0.,-1.,0.));
#5506=DIRECTION('ref_axis',(-1.,0.,0.));
#5507=DIRECTION('axis',(0.,0.,1.));
#5508=DIRECTION('refdir',(1.,0.,0.));
#5509=DIRECTION('',(0.,0.,1.));
#5510=DIRECTION('',(0.,0.,1.));
#5511=DIRECTION('',(0.,8.75964579554923E-17,-1.));
#5512=DIRECTION('',(0.,0.,-1.));
#5513=DIRECTION('center_axis',(0.,-1.,0.));
#5514=DIRECTION('ref_axis',(1.,0.,0.));
#5515=DIRECTION('center_axis',(0.,-1.,0.));
#5516=DIRECTION('ref_axis',(1.,0.,0.));
#5517=DIRECTION('',(-1.,0.,0.));
#5518=DIRECTION('',(1.,0.,0.));
#5519=DIRECTION('',(-1.,0.,0.));
#5520=DIRECTION('center_axis',(0.,1.,0.));
#5521=DIRECTION('ref_axis',(0.918783056912983,0.,-0.3947628330145));
#5522=DIRECTION('center_axis',(0.,-1.,0.));
#5523=DIRECTION('ref_axis',(1.,0.,0.));
#5524=DIRECTION('',(0.,0.,1.));
#5525=DIRECTION('center_axis',(0.,1.,0.));
#5526=DIRECTION('ref_axis',(1.,0.,0.));
#5527=DIRECTION('center_axis',(0.,1.,0.));
#5528=DIRECTION('ref_axis',(1.,0.,0.));
#5529=DIRECTION('center_axis',(0.,-1.,0.));
#5530=DIRECTION('ref_axis',(1.,0.,0.));
#5531=DIRECTION('',(1.,0.,0.));
#5532=DIRECTION('',(0.,0.,1.));
#5533=DIRECTION('',(-1.,0.,0.));
#5534=DIRECTION('center_axis',(-1.,0.,0.));
#5535=DIRECTION('ref_axis',(0.,-1.,0.));
#5536=DIRECTION('',(0.,-1.,0.));
#5537=DIRECTION('',(0.,0.,1.));
#5538=DIRECTION('',(0.,1.,0.));
#5539=DIRECTION('',(0.,0.,1.));
#5540=DIRECTION('center_axis',(0.,1.,0.));
#5541=DIRECTION('ref_axis',(-1.,0.,0.));
#5542=DIRECTION('',(-1.,0.,0.));
#5543=DIRECTION('',(1.,0.,0.));
#5544=DIRECTION('',(0.,0.,-1.));
#5545=DIRECTION('center_axis',(0.,0.,1.));
#5546=DIRECTION('ref_axis',(1.,0.,0.));
#5547=DIRECTION('',(0.,-1.,0.));
#5548=DIRECTION('',(1.,0.,0.));
#5549=DIRECTION('',(1.,0.,0.));
#5550=DIRECTION('center_axis',(0.,0.,1.));
#5551=DIRECTION('ref_axis',(1.,0.,0.));
#5552=DIRECTION('center_axis',(0.,0.,1.));
#5553=DIRECTION('ref_axis',(1.,0.,0.));
#5554=DIRECTION('',(0.,1.,0.));
#5555=DIRECTION('',(-1.,0.,0.));
#5556=DIRECTION('',(0.,1.,0.));
#5557=DIRECTION('center_axis',(0.,0.,1.));
#5558=DIRECTION('ref_axis',(1.,0.,0.));
#5559=DIRECTION('',(0.,-1.,0.));
#5560=DIRECTION('',(-1.,0.,0.));
#5561=DIRECTION('center_axis',(0.,1.,0.));
#5562=DIRECTION('ref_axis',(1.,0.,0.));
#5563=DIRECTION('',(0.,1.,0.));
#5564=DIRECTION('center_axis',(0.,-1.,0.));
#5565=DIRECTION('ref_axis',(1.,0.,0.));
#5566=DIRECTION('center_axis',(0.,1.,0.));
#5567=DIRECTION('ref_axis',(1.,0.,0.));
#5568=DIRECTION('',(0.,-1.,0.));
#5569=DIRECTION('center_axis',(0.,-1.,0.));
#5570=DIRECTION('ref_axis',(1.,0.,0.));
#5571=DIRECTION('',(0.,-1.,0.));
#5572=DIRECTION('center_axis',(0.,1.,0.));
#5573=DIRECTION('ref_axis',(0.918783056912983,0.,-0.3947628330145));
#5574=DIRECTION('',(0.,-1.,0.));
#5575=DIRECTION('center_axis',(0.,1.,0.));
#5576=DIRECTION('ref_axis',(0.918783056912983,0.,-0.3947628330145));
#5577=DIRECTION('center_axis',(0.,0.,-1.));
#5578=DIRECTION('ref_axis',(-1.,0.,0.));
#5579=DIRECTION('center_axis',(0.,0.,-1.));
#5580=DIRECTION('ref_axis',(1.,0.,0.));
#5581=DIRECTION('',(-1.,0.,0.));
#5582=DIRECTION('',(-1.,0.,0.));
#5583=DIRECTION('',(1.,0.,0.));
#5584=DIRECTION('',(0.,-1.,0.));
#5585=DIRECTION('center_axis',(0.,0.,-1.));
#5586=DIRECTION('ref_axis',(1.,0.,0.));
#5587=DIRECTION('center_axis',(0.,1.,0.));
#5588=DIRECTION('ref_axis',(1.,0.,0.));
#5589=DIRECTION('center_axis',(0.,1.,0.));
#5590=DIRECTION('ref_axis',(1.,0.,0.));
#5591=DIRECTION('',(0.,1.,0.));
#5592=DIRECTION('center_axis',(0.,1.,0.));
#5593=DIRECTION('ref_axis',(1.,0.,0.));
#5594=DIRECTION('center_axis',(0.,1.,0.));
#5595=DIRECTION('ref_axis',(1.,0.,0.));
#5596=DIRECTION('',(0.,1.,0.));
#5597=DIRECTION('center_axis',(1.,0.,0.));
#5598=DIRECTION('ref_axis',(0.,1.,0.));
#5599=DIRECTION('',(0.,0.,1.));
#5600=DIRECTION('',(0.,0.,1.));
#5601=DIRECTION('',(0.,0.,1.));
#5602=DIRECTION('center_axis',(0.,-1.,0.));
#5603=DIRECTION('ref_axis',(1.,0.,0.));
#5604=DIRECTION('center_axis',(0.,-1.,0.));
#5605=DIRECTION('ref_axis',(1.,0.,0.));
#5606=DIRECTION('',(0.,0.,1.));
#5607=DIRECTION('center_axis',(0.,0.,1.));
#5608=DIRECTION('ref_axis',(-1.,1.22464679914735E-16,0.));
#5609=DIRECTION('center_axis',(0.,0.,1.));
#5610=DIRECTION('ref_axis',(-1.,1.22464679914735E-16,0.));
#5611=DIRECTION('',(0.,0.,1.));
#5612=DIRECTION('center_axis',(1.,0.,0.));
#5613=DIRECTION('ref_axis',(0.,1.,0.));
#5614=DIRECTION('',(0.,0.,1.));
#5615=DIRECTION('center_axis',(0.,1.,0.));
#5616=DIRECTION('ref_axis',(-1.,0.,0.));
#5617=DIRECTION('axis',(0.,0.,1.));
#5618=DIRECTION('refdir',(1.,0.,0.));
#5619=DIRECTION('center_axis',(0.,1.,0.));
#5620=DIRECTION('ref_axis',(-0.940813565885044,0.,-0.338924525885436));
#5621=DIRECTION('center_axis',(-0.338924525885436,8.35610306180218E-15,
0.940813565885044));
#5622=DIRECTION('ref_axis',(2.13510934712592E-31,1.,-8.88178419700125E-15));
#5623=DIRECTION('center_axis',(0.,1.,0.));
#5624=DIRECTION('ref_axis',(-0.0570391179197161,0.,0.998371944230676));
#5625=DIRECTION('center_axis',(-0.338924525885436,-8.35610306180218E-15,
0.940813565885044));
#5626=DIRECTION('ref_axis',(-0.940813565885044,-4.28735023454931E-31,-0.338924525885436));
#5627=DIRECTION('center_axis',(0.,-1.,0.));
#5628=DIRECTION('ref_axis',(0.0203769416068415,0.,0.99979236856997));
#5629=DIRECTION('center_axis',(0.,-1.,0.));
#5630=DIRECTION('ref_axis',(0.0570391179197162,0.,-0.998371944230676));
#5631=DIRECTION('center_axis',(0.338924525885434,0.,-0.940813565885045));
#5632=DIRECTION('ref_axis',(-0.66525565226961,-0.70710678118655,-0.239655830564025));
#5633=DIRECTION('center_axis',(-0.338924525885432,0.,0.940813565885046));
#5634=DIRECTION('ref_axis',(-0.940813565885046,0.,-0.338924525885432));
#5635=DIRECTION('',(-0.338924525885434,0.,0.940813565885045));
#5636=DIRECTION('',(0.338924525885434,0.,-0.940813565885045));
#5637=DIRECTION('center_axis',(0.,-1.,0.));
#5638=DIRECTION('ref_axis',(-0.940813565885045,0.,-0.338924525885434));
#5639=DIRECTION('center_axis',(0.,-1.,0.));
#5640=DIRECTION('ref_axis',(-0.555722380368519,0.,-0.83136793055635));
#5641=DIRECTION('center_axis',(0.,-1.,0.));
#5642=DIRECTION('ref_axis',(-0.940813565885044,0.,-0.338924525885436));
#5643=DIRECTION('',(0.,-1.,0.));
#5644=DIRECTION('',(0.,1.,0.));
#5645=DIRECTION('center_axis',(0.338924525885437,-2.61128220681318E-15,
-0.940813565885044));
#5646=DIRECTION('ref_axis',(-0.940813565885044,4.44089209850066E-15,-0.338924525885437));
#5647=DIRECTION('center_axis',(0.338924525885434,0.,-0.940813565885045));
#5648=DIRECTION('ref_axis',(-0.665255652269609,0.707106781186551,-0.239655830564025));
#5649=DIRECTION('',(-0.338924525885434,0.,0.940813565885045));
#5650=DIRECTION('',(0.338924525885434,0.,-0.940813565885045));
#5651=DIRECTION('center_axis',(0.,1.,0.));
#5652=DIRECTION('ref_axis',(-0.812306361973871,0.,0.583230978512608));
#5653=DIRECTION('',(0.,-1.,0.));
#5654=DIRECTION('',(0.,1.,0.));
#5655=DIRECTION('center_axis',(0.,-1.,0.));
#5656=DIRECTION('ref_axis',(1.,0.,0.));
#5657=DIRECTION('center_axis',(0.,1.,0.));
#5658=DIRECTION('ref_axis',(0.141943234522443,0.,-0.989874799241453));
#5659=DIRECTION('',(4.67836035237689E-14,0.,1.));
#5660=DIRECTION('center_axis',(0.,-1.,0.));
#5661=DIRECTION('ref_axis',(0.335988807373518,0.,-0.941865978427781));
#5662=DIRECTION('center_axis',(0.,1.,0.));
#5663=DIRECTION('ref_axis',(0.147769932247684,0.,-0.989021762714813));
#5664=DIRECTION('center_axis',(0.,-1.,0.));
#5665=DIRECTION('ref_axis',(0.141943234522443,0.,-0.989874799241453));
#5666=DIRECTION('center_axis',(-0.950173445040706,-4.15296743349361E-15,
-0.31172170976606));
#5667=DIRECTION('ref_axis',(-0.31172170976606,-2.25212199954037E-32,0.950173445040706));
#5668=DIRECTION('center_axis',(0.,-1.,0.));
#5669=DIRECTION('ref_axis',(-0.032150446799728,0.,-0.999483040761862));
#5670=DIRECTION('center_axis',(0.,1.,0.));
#5671=DIRECTION('ref_axis',(0.141943234522443,0.,-0.989874799241453));
#5672=DIRECTION('',(0.,-1.,0.));
#5673=DIRECTION('center_axis',(0.,1.,0.));
#5674=DIRECTION('ref_axis',(0.147769932247684,0.,-0.989021762714813));
#5675=DIRECTION('center_axis',(0.,-1.,0.));
#5676=DIRECTION('ref_axis',(0.141943234522443,0.,-0.989874799241453));
#5677=DIRECTION('center_axis',(-0.950173445040706,1.3843224778312E-15,-0.31172170976606));
#5678=DIRECTION('ref_axis',(2.67362611073496E-30,-1.,-4.44089209850063E-15));
#5679=DIRECTION('center_axis',(-0.940813565885045,0.,-0.338924525885434));
#5680=DIRECTION('ref_axis',(0.338924525885434,0.,-0.940813565885045));
#5681=DIRECTION('',(0.338924525885434,0.,-0.940813565885045));
#5682=DIRECTION('',(0.,1.,0.));
#5683=DIRECTION('',(0.338924525885434,0.,-0.940813565885045));
#5684=DIRECTION('center_axis',(-0.944875085787754,-5.26189473139136E-12,
-0.327431019082774));
#5685=DIRECTION('ref_axis',(0.327431019082774,4.11381421934135E-29,-0.944875085787754));
#5686=DIRECTION('center_axis',(0.,0.,1.));
#5687=DIRECTION('ref_axis',(1.,0.,0.));
#5688=DIRECTION('center_axis',(0.,-1.,0.));
#5689=DIRECTION('ref_axis',(1.,0.,-4.66293670342563E-14));
#5690=DIRECTION('center_axis',(-4.67836035237689E-14,0.,-1.));
#5691=DIRECTION('ref_axis',(0.707106781186546,-0.707106781186549,-3.30810032999998E-14));
#5692=DIRECTION('center_axis',(0.,-1.,0.));
#5693=DIRECTION('ref_axis',(0.,0.,-1.));
#5694=DIRECTION('center_axis',(0.,-1.,0.));
#5695=DIRECTION('ref_axis',(0.335988807373518,0.,-0.941865978427781));
#5696=DIRECTION('center_axis',(0.,1.,0.));
#5697=DIRECTION('ref_axis',(0.335988807373518,0.,-0.941865978427781));
#5698=DIRECTION('center_axis',(4.67836035237689E-14,0.,1.));
#5699=DIRECTION('ref_axis',(0.707106781186546,-0.707106781186549,-3.30810032999998E-14));
#5700=DIRECTION('',(4.67836035237689E-14,0.,1.));
#5701=DIRECTION('center_axis',(4.67836035237689E-14,0.,1.));
#5702=DIRECTION('ref_axis',(0.707106781186546,-0.707106781186549,-3.30810032999998E-14));
#5703=DIRECTION('',(-4.67836035237689E-14,0.,-1.));
#5704=DIRECTION('',(0.,1.,0.));
#5705=DIRECTION('center_axis',(0.,1.,0.));
#5706=DIRECTION('ref_axis',(1.,0.,-4.66293670342563E-14));
#5707=DIRECTION('',(0.,-1.,0.));
#5708=DIRECTION('',(0.,-1.,0.));
#5709=DIRECTION('center_axis',(-0.894799777334527,-0.323660756971229,0.307533856475823));
#5710=DIRECTION('ref_axis',(0.446467645504215,-0.648673148404086,0.616352000124485));
#5711=DIRECTION('center_axis',(0.,-1.,0.));
#5712=DIRECTION('ref_axis',(0.586633740179502,0.,0.809852366103235));
#5713=DIRECTION('center_axis',(0.,-1.,0.));
#5714=DIRECTION('ref_axis',(1.,0.,0.));
#5715=DIRECTION('center_axis',(0.,-1.,0.));
#5716=DIRECTION('ref_axis',(0.,0.,-1.));
#5717=DIRECTION('center_axis',(0.,1.,0.));
#5718=DIRECTION('ref_axis',(0.335988807373518,0.,-0.941865978427781));
#5719=DIRECTION('center_axis',(-0.944875085789614,0.,-0.327431019077409));
#5720=DIRECTION('ref_axis',(0.,1.,0.));
#5721=DIRECTION('center_axis',(0.,0.,1.));
#5722=DIRECTION('ref_axis',(1.,0.,0.));
#5723=DIRECTION('center_axis',(-4.67836035237689E-14,0.,-1.));
#5724=DIRECTION('ref_axis',(0.707106781186546,0.707106781186549,-3.30810032999998E-14));
#5725=DIRECTION('center_axis',(4.67836035237689E-14,0.,1.));
#5726=DIRECTION('ref_axis',(0.707106781186546,0.707106781186549,-3.30810032999998E-14));
#5727=DIRECTION('center_axis',(4.67836035237689E-14,0.,1.));
#5728=DIRECTION('ref_axis',(0.707106781186546,0.707106781186549,-3.30810032999998E-14));
#5729=DIRECTION('',(-4.67836035237689E-14,0.,-1.));
#5730=DIRECTION('center_axis',(-0.894799777334522,0.323660756971238,0.307533856475827));
#5731=DIRECTION('ref_axis',(0.446467645504229,0.648673148404085,0.616352000124476));
#5732=DIRECTION('center_axis',(0.,1.,0.));
#5733=DIRECTION('ref_axis',(0.586633740179502,0.,0.809852366103235));
#5734=DIRECTION('center_axis',(0.,-1.,0.));
#5735=DIRECTION('ref_axis',(0.586633740179504,0.,0.809852366103234));
#5736=DIRECTION('',(0.,1.,0.));
#5737=DIRECTION('center_axis',(1.,0.,-4.67836035237689E-14));
#5738=DIRECTION('ref_axis',(4.67836035237689E-14,0.,1.));
#5739=DIRECTION('center_axis',(0.,-1.,0.));
#5740=DIRECTION('ref_axis',(1.,0.,0.));
#5741=DIRECTION('',(-4.18364780870191E-14,0.,-1.));
#5742=DIRECTION('center_axis',(0.,-1.,0.));
#5743=DIRECTION('ref_axis',(-0.032150677597388,0.,-0.999483033337749));
#5744=DIRECTION('center_axis',(0.,1.,0.));
#5745=DIRECTION('ref_axis',(-0.032150677597388,0.,-0.999483033337749));
#5746=DIRECTION('',(0.,1.,0.));
#5747=DIRECTION('center_axis',(0.,-1.,0.));
#5748=DIRECTION('ref_axis',(-0.032150677597388,0.,-0.999483033337749));
#5749=DIRECTION('center_axis',(-1.,0.,4.18364780870191E-14));
#5750=DIRECTION('ref_axis',(4.18364780870191E-14,0.,1.));
#5751=DIRECTION('',(0.,1.,0.));
#5752=DIRECTION('',(-4.18364780870191E-14,0.,-1.));
#5753=DIRECTION('center_axis',(0.,-1.,0.));
#5754=DIRECTION('ref_axis',(1.,0.,0.));
#5755=DIRECTION('center_axis',(0.,-1.,0.));
#5756=DIRECTION('ref_axis',(0.0278513911097204,0.,-0.999612074763632));
#5757=DIRECTION('',(0.,0.,1.));
#5758=DIRECTION('',(1.,0.,0.));
#5759=DIRECTION('',(0.,0.,1.));
#5760=DIRECTION('',(1.,0.,0.));
#5761=DIRECTION('',(0.,0.,1.));
#5762=DIRECTION('',(1.,0.,0.));
#5763=DIRECTION('',(0.,0.,1.));
#5764=DIRECTION('',(1.,0.,0.));
#5765=DIRECTION('',(0.,0.,1.));
#5766=DIRECTION('',(1.,0.,0.));
#5767=DIRECTION('',(0.,0.,1.));
#5768=DIRECTION('',(1.,0.,0.));
#5769=DIRECTION('',(0.,0.,1.));
#5770=DIRECTION('',(1.,0.,0.));
#5771=DIRECTION('',(0.,0.,1.));
#5772=DIRECTION('',(1.,0.,0.));
#5773=DIRECTION('',(0.,0.,1.));
#5774=DIRECTION('',(1.,0.,0.));
#5775=CARTESIAN_POINT('',(0.,0.,0.));
#5776=CARTESIAN_POINT('',(0.,0.,0.));
#5777=CARTESIAN_POINT('Origin',(37.3390884548007,1.63165946910082,-0.451167579126729));
#5778=CARTESIAN_POINT('',(35.5793396636553,1.63165946910082,-0.45116757912673));
#5779=CARTESIAN_POINT('Origin',(37.3390884548007,1.63165946910082,-0.451167579126729));
#5780=CARTESIAN_POINT('',(35.5793396636553,-1.63134053089918,-0.451167579126729));
#5781=CARTESIAN_POINT('',(35.5793396636553,1.63165946910082,-0.451167579126729));
#5782=CARTESIAN_POINT('Origin',(37.3390884548007,-1.63134053089918,-0.451167579126729));
#5783=CARTESIAN_POINT('Origin',(32.143405418954,1.63165946910082,3.2164639050219));
#5784=CARTESIAN_POINT('',(30.4486229160323,1.63165946910082,3.2164639050219));
#5785=CARTESIAN_POINT('Origin',(32.143405418954,1.63165946910082,3.2164639050219));
#5786=CARTESIAN_POINT('',(30.4486229160323,-1.63134053089918,3.2164639050219));
#5787=CARTESIAN_POINT('',(30.4486229160323,1.63165946910082,3.2164639050219));
#5788=CARTESIAN_POINT('Origin',(32.143405418954,-1.63134053089918,3.2164639050219));
#5789=CARTESIAN_POINT('Origin',(37.3390884548007,1.63165946910082,-0.451167579126729));
#5790=CARTESIAN_POINT('',(36.1646139528278,1.63165946910082,-2.38173077242002));
#5791=CARTESIAN_POINT('',(38.6217323111757,1.63165946910082,1.40928648824138));
#5792=CARTESIAN_POINT('Origin',(37.3390884548007,1.63165946910082,-0.451167579126729));
#5793=CARTESIAN_POINT('',(38.6217323111757,-1.63134053089918,1.40928648824138));
#5794=CARTESIAN_POINT('',(38.6217323111757,1.63165946910082,1.40928648824138));
#5795=CARTESIAN_POINT('',(36.1646139528278,-1.63134053089918,-2.38173077242002));
#5796=CARTESIAN_POINT('Origin',(37.3390884548007,-1.63134053089918,-0.451167579126729));
#5797=CARTESIAN_POINT('',(36.1646139528278,1.63165946910082,-2.38173077242002));
#5798=CARTESIAN_POINT('Origin',(30.6537580146004,1.63165946910082,0.970845204361578));
#5799=CARTESIAN_POINT('',(30.6537580146004,1.63165946910082,0.970845204361578));
#5800=CARTESIAN_POINT('',(30.6537580146004,1.63165946910082,0.970845204361578));
#5801=CARTESIAN_POINT('',(30.6537580146004,-1.63134053089918,0.970845204361578));
#5802=CARTESIAN_POINT('',(30.6537580146004,-1.63134053089918,0.970845204361578));
#5803=CARTESIAN_POINT('',(30.6537580146004,1.63165946910082,0.970845204361578));
#5804=CARTESIAN_POINT('Origin',(32.143405418954,1.63165946910082,3.2164639050219));
#5805=CARTESIAN_POINT('',(33.84684183669,1.63165946910082,5.30456282719571));
#5806=CARTESIAN_POINT('Origin',(32.143405418954,1.63165946910082,3.2164639050219));
#5807=CARTESIAN_POINT('',(33.84684183669,-1.63134053089918,5.30456282719571));
#5808=CARTESIAN_POINT('Origin',(32.143405418954,-1.63134053089918,3.2164639050219));
#5809=CARTESIAN_POINT('',(33.84684183669,1.63165946910082,5.30456282719571));
#5810=CARTESIAN_POINT('Origin',(38.6217323111757,1.63165946910082,1.40928648824138));
#5811=CARTESIAN_POINT('',(38.6217323111757,1.63165946910082,1.40928648824138));
#5812=CARTESIAN_POINT('',(38.6217323111757,-1.63134053089918,1.40928648824138));
#5813=CARTESIAN_POINT('Origin',(34.5237300809892,-1.63134053089918,1.60016501883572));
#5814=CARTESIAN_POINT('Origin',(34.5237300809892,1.63165946910082,1.60016501883572));
#5815=CARTESIAN_POINT('',(0.,0.,0.));
#5816=CARTESIAN_POINT('Origin',(24.7143466872546,-3.13165946910082,-0.395297377936459));
#5817=CARTESIAN_POINT('',(24.7143466872546,-3.63165946910083,1.30603779103116));
#5818=CARTESIAN_POINT('Origin',(24.7143466872546,-3.63165946910082,-0.395297377936459));
#5819=CARTESIAN_POINT('',(24.7143466872546,-3.13165946910082,1.80603779103116));
#5820=CARTESIAN_POINT('Origin',(24.7143466872546,-3.13165946910082,1.30603779103116));
#5821=CARTESIAN_POINT('Origin',(24.7143466872546,-3.13165946910082,-0.395297377936459));
#5822=CARTESIAN_POINT('Origin',(24.7143466872546,-3.63165946910082,-0.395297377936459));
#5823=CARTESIAN_POINT('Origin',(37.3390884548007,-3.13165946910082,-0.451167579126729));
#5824=CARTESIAN_POINT('',(37.3390884548007,-3.63165946910083,1.30858121201868));
#5825=CARTESIAN_POINT('Origin',(37.3390884548007,-3.63165946910082,-0.451167579126729));
#5826=CARTESIAN_POINT('',(37.3390884548007,-3.13165946910082,1.80858121201868));
#5827=CARTESIAN_POINT('Origin',(37.3390884548007,-3.13165946910082,1.30858121201868));
#5828=CARTESIAN_POINT('Origin',(37.3390884548007,-3.13165946910082,-0.451167579126729));
#5829=CARTESIAN_POINT('Origin',(37.3390884548007,-3.63165946910082,-0.451167579126729));
#5830=CARTESIAN_POINT('Origin',(25.1607982446856,-4.63165946910082,-5.));
#5831=CARTESIAN_POINT('',(19.2071026744088,-4.63165946910082,-6.5));
#5832=CARTESIAN_POINT('',(19.8239560216472,-3.13165946910082,-5.));
#5833=CARTESIAN_POINT('Origin',(19.8239560216472,-4.63165946910082,-5.));
#5834=CARTESIAN_POINT('',(43.0218849555161,-4.63165946910082,-6.5));
#5835=CARTESIAN_POINT('',(25.1607982446856,-4.63165946910082,-6.5));
#5836=CARTESIAN_POINT('',(42.4050316082777,-3.13165946910082,-5.));
#5837=CARTESIAN_POINT('Origin',(42.4050316082777,-4.63165946910082,-5.));
#5838=CARTESIAN_POINT('',(25.1607982446856,-3.13165946910082,-5.));
#5839=CARTESIAN_POINT('Origin',(19.2071026744088,-3.13165946910082,-8.5));
#5840=CARTESIAN_POINT('',(40.0215468039921,-3.13165946910082,0.79591117148755));
#5841=CARTESIAN_POINT('',(41.6512074608448,-3.13165946910082,-3.16692861243009));
#5842=CARTESIAN_POINT('',(37.4782084817555,-3.13165946910082,2.5));
#5843=CARTESIAN_POINT('Origin',(37.4782084817555,-3.13165946910082,-0.25));
#5844=CARTESIAN_POINT('',(37.2590007645168,-3.13165946910082,2.5));
#5845=CARTESIAN_POINT('',(19.2071026744088,-3.13165946910082,2.5));
#5846=CARTESIAN_POINT('',(34.7590007645168,-3.13165946910082,0.));
#5847=CARTESIAN_POINT('Origin',(37.2590007645168,-3.13165946910082,0.));
#5848=CARTESIAN_POINT('',(34.7590007645168,-3.13165946910082,-0.758936728277321));
#5849=CARTESIAN_POINT('',(34.7590007645168,-3.13165946910082,-3.));
#5850=CARTESIAN_POINT('',(34.6904980837498,-3.13165946910082,-1.277895402736));
#5851=CARTESIAN_POINT('Origin',(32.7590007645165,-3.13165946910082,-0.758936728277284));
#5852=CARTESIAN_POINT('',(27.5384895461752,-3.13165946910082,-1.277895402736));
#5853=CARTESIAN_POINT('Origin',(31.1144938149625,-3.13165946910082,-0.317087216926334));
#5854=CARTESIAN_POINT('',(27.4699868654081,-3.13165946910082,-0.758936728277321));
#5855=CARTESIAN_POINT('Origin',(29.4699868654084,-3.13165946910082,-0.758936728277284));
#5856=CARTESIAN_POINT('',(27.4699868654081,-3.13165946910082,0.));
#5857=CARTESIAN_POINT('',(27.4699868654081,-3.13165946910082,-4.62946836413866));
#5858=CARTESIAN_POINT('',(24.9699868654081,-3.13165946910082,2.5));
#5859=CARTESIAN_POINT('Origin',(24.9699868654081,-3.13165946910082,0.));
#5860=CARTESIAN_POINT('',(24.7507791481694,-3.13165946910082,2.5));
#5861=CARTESIAN_POINT('',(19.2071026744088,-3.13165946910082,2.5));
#5862=CARTESIAN_POINT('',(22.2074408259328,-3.13165946910082,0.795911171487552));
#5863=CARTESIAN_POINT('Origin',(24.7507791481694,-3.13165946910082,-0.25));
#5864=CARTESIAN_POINT('',(20.7059131671521,-3.13165946910082,-2.85534807555141));
#5865=CARTESIAN_POINT('Origin',(37.2590007645168,-2.75665946910082,0.));
#5866=CARTESIAN_POINT('',(37.2590007645168,-1.63165946910082,2.5));
#5867=CARTESIAN_POINT('',(37.2590007645168,-2.75665946910082,2.5));
#5868=CARTESIAN_POINT('',(34.7590007645168,-1.63165946910082,0.));
#5869=CARTESIAN_POINT('Origin',(37.2590007645168,-1.63165946910082,0.));
#5870=CARTESIAN_POINT('',(34.7590007645168,-2.75665946910082,0.));
#5871=CARTESIAN_POINT('Origin',(31.1144938149625,-2.38165946910082,2.5));
#5872=CARTESIAN_POINT('',(37.4782084817555,-1.63165946910082,2.5));
#5873=CARTESIAN_POINT('',(37.4782084817555,-2.75665946910082,2.5));
#5874=CARTESIAN_POINT('',(43.0218849555161,-1.63165946910082,2.5));
#5875=CARTESIAN_POINT('Origin',(24.9699868654081,-2.75665946910082,0.));
#5876=CARTESIAN_POINT('',(27.4699868654081,-1.63165946910082,0.));
#5877=CARTESIAN_POINT('',(24.9699868654081,-1.63165946910082,2.5));
#5878=CARTESIAN_POINT('Origin',(24.9699868654081,-1.63165946910082,0.));
#5879=CARTESIAN_POINT('',(24.9699868654081,-2.75665946910082,2.5));
#5880=CARTESIAN_POINT('',(27.4699868654081,-2.75665946910082,0.));
#5881=CARTESIAN_POINT('Origin',(27.4699868654081,-3.13165946910082,-0.758936728277321));
#5882=CARTESIAN_POINT('',(27.4699868654081,-1.63165946910082,-0.758936728277321));
#5883=CARTESIAN_POINT('',(27.4699868654081,-3.13165946910082,-0.758936728277321));
#5884=CARTESIAN_POINT('',(27.4699868654081,-1.63165946910082,-4.62946836413866));
#5885=CARTESIAN_POINT('Origin',(37.4782084817555,-2.75665946910082,-0.25));
#5886=CARTESIAN_POINT('',(40.0215468039921,-1.63165946910082,0.795911171487551));
#5887=CARTESIAN_POINT('Origin',(37.4782084817555,-1.63165946910082,-0.25));
#5888=CARTESIAN_POINT('',(40.0215468039921,-2.75665946910082,0.795911171487553));
#5889=CARTESIAN_POINT('Origin',(43.0218849555161,-3.13165946910082,-6.5));
#5890=CARTESIAN_POINT('',(43.0218849555161,-1.63165946910082,-6.5));
#5891=CARTESIAN_POINT('',(43.0218849555161,-3.13165946910082,-6.5));
#5892=CARTESIAN_POINT('',(43.373634504488,-1.63165946910082,-7.35534807555141));
#5893=CARTESIAN_POINT('Origin',(24.7507791481694,-2.75665946910082,-0.25));
#5894=CARTESIAN_POINT('',(24.7507791481694,-1.63165946910082,2.5));
#5895=CARTESIAN_POINT('',(24.7507791481694,-2.75665946910082,2.5));
#5896=CARTESIAN_POINT('',(22.2074408259328,-1.63165946910082,0.795911171487552));
#5897=CARTESIAN_POINT('Origin',(24.7507791481694,-1.63165946910082,-0.25));
#5898=CARTESIAN_POINT('',(22.2074408259328,-2.75665946910082,0.795911171487551));
#5899=CARTESIAN_POINT('Origin',(22.9082227578391,-3.13165946910082,2.5));
#5900=CARTESIAN_POINT('',(19.2071026744088,-1.63165946910082,-6.5));
#5901=CARTESIAN_POINT('',(22.4283402107953,-1.63165946910082,1.3330713875699));
#5902=CARTESIAN_POINT('',(19.2071026744088,-9.4502026108178,-6.5));
#5903=CARTESIAN_POINT('Origin',(32.7590007645165,-3.13165946910082,-0.758936728277284));
#5904=CARTESIAN_POINT('',(34.6904980837498,-1.63165946910082,-1.277895402736));
#5905=CARTESIAN_POINT('',(34.7590007645168,-1.63165946910082,-0.758936728277321));
#5906=CARTESIAN_POINT('Origin',(32.7590007645165,-1.63165946910082,-0.758936728277284));
#5907=CARTESIAN_POINT('',(34.6904980837498,-3.13165946910082,-1.277895402736));
#5908=CARTESIAN_POINT('',(34.7590007645168,-3.13165946910082,-0.758936728277321));
#5909=CARTESIAN_POINT('Origin',(34.7590007645168,-3.13165946910082,2.5));
#5910=CARTESIAN_POINT('',(34.7590007645168,-1.63165946910082,-3.));
#5911=CARTESIAN_POINT('Origin',(29.4699868654084,-3.13165946910082,-0.758936728277284));
#5912=CARTESIAN_POINT('',(27.5384895461752,-1.63165946910082,-1.277895402736));
#5913=CARTESIAN_POINT('Origin',(29.4699868654084,-1.63165946910082,-0.758936728277284));
#5914=CARTESIAN_POINT('',(27.5384895461752,-3.13165946910082,-1.277895402736));
#5915=CARTESIAN_POINT('Origin',(31.1144938149625,-3.13165946910082,-0.317087216926334));
#5916=CARTESIAN_POINT('Origin',(31.1144938149625,-1.63165946910082,-0.317087216926334));
#5917=CARTESIAN_POINT('Origin',(43.0218849555161,-9.4502026108178,-8.5));
#5918=CARTESIAN_POINT('',(43.0218849555161,-9.4502026108178,-6.5));
#5919=CARTESIAN_POINT('',(43.0218849555161,-3.13165946910082,-6.5));
#5920=CARTESIAN_POINT('',(43.0218849555161,-9.4502026108178,-8.5));
#5921=CARTESIAN_POINT('',(43.0218849555161,-9.4502026108178,-8.5));
#5922=CARTESIAN_POINT('',(43.0218849555161,-1.63165946910082,-8.5));
#5923=CARTESIAN_POINT('',(43.0218849555161,-3.13165946910082,-8.5));
#5924=CARTESIAN_POINT('',(43.0218849555161,-1.63165946910082,-8.5));
#5925=CARTESIAN_POINT('Origin',(43.0218849555161,-1.63165946910082,-8.5));
#5926=CARTESIAN_POINT('',(19.2071026744088,-1.63165946910082,-8.5));
#5927=CARTESIAN_POINT('',(43.0218849555161,-1.63165946910082,-8.5));
#5928=CARTESIAN_POINT('',(19.2071026744088,-1.63165946910082,-8.5));
#5929=CARTESIAN_POINT('',(43.0218849555161,-1.63165946910082,2.5));
#5930=CARTESIAN_POINT('Origin',(31.1144938149625,-2.38165946910082,2.5));
#5931=CARTESIAN_POINT('Origin',(38.9466240721952,-10.3406188648021,-8.5));
#5932=CARTESIAN_POINT('',(38.9466240721952,-10.3406188648021,-8.5));
#5933=CARTESIAN_POINT('',(36.8121029357457,-10.3406188648021,-8.5));
#5934=CARTESIAN_POINT('',(36.8121029357457,-10.3406188648021,-8.5));
#5935=CARTESIAN_POINT('',(36.8121029357457,-10.3406188648021,-6.5));
#5936=CARTESIAN_POINT('',(36.8121029357457,-10.3406188648021,-8.5));
#5937=CARTESIAN_POINT('',(38.9466240721952,-10.3406188648021,-6.5));
#5938=CARTESIAN_POINT('',(36.8121029357457,-10.3406188648021,-6.5));
#5939=CARTESIAN_POINT('',(38.9466240721952,-10.3406188648021,-8.5));
#5940=CARTESIAN_POINT('Origin',(38.9466240721952,-8.04398219900198,-8.5));
#5941=CARTESIAN_POINT('',(38.9466240721952,-5.74734553320186,-8.5));
#5942=CARTESIAN_POINT('Origin',(38.9466240721952,-8.04398219900198,-8.5));
#5943=CARTESIAN_POINT('',(38.9466240721952,-5.74734553320186,-6.5));
#5944=CARTESIAN_POINT('Origin',(38.9466240721952,-8.04398219900198,-6.5));
#5945=CARTESIAN_POINT('',(38.9466240721952,-5.74734553320186,-8.5));
#5946=CARTESIAN_POINT('Origin',(36.8121029357457,-5.74734553320186,-8.5));
#5947=CARTESIAN_POINT('',(36.8121029357457,-5.74734553320186,-8.5));
#5948=CARTESIAN_POINT('',(38.9466240721952,-5.74734553320186,-8.5));
#5949=CARTESIAN_POINT('',(36.8121029357457,-5.74734553320186,-6.5));
#5950=CARTESIAN_POINT('',(38.9466240721952,-5.74734553320186,-6.5));
#5951=CARTESIAN_POINT('',(36.8121029357457,-5.74734553320186,-8.5));
#5952=CARTESIAN_POINT('Origin',(36.8121029357457,-8.04398219900198,-8.5));
#5953=CARTESIAN_POINT('Origin',(36.8121029357457,-8.04398219900198,-8.5));
#5954=CARTESIAN_POINT('Origin',(36.8121029357457,-8.04398219900198,-6.5));
#5955=CARTESIAN_POINT('Origin',(25.4466240721952,-10.3406188648021,-8.5));
#5956=CARTESIAN_POINT('',(25.4466240721952,-10.3406188648021,-8.5));
#5957=CARTESIAN_POINT('',(23.3121029357457,-10.3406188648021,-8.5));
#5958=CARTESIAN_POINT('',(23.3121029357457,-10.3406188648021,-8.5));
#5959=CARTESIAN_POINT('',(23.3121029357457,-10.3406188648021,-6.5));
#5960=CARTESIAN_POINT('',(23.3121029357457,-10.3406188648021,-8.5));
#5961=CARTESIAN_POINT('',(25.4466240721952,-10.3406188648021,-6.5));
#5962=CARTESIAN_POINT('',(23.3121029357457,-10.3406188648021,-6.5));
#5963=CARTESIAN_POINT('',(25.4466240721952,-10.3406188648021,-8.5));
#5964=CARTESIAN_POINT('Origin',(25.4466240721952,-8.04398219900198,-8.5));
#5965=CARTESIAN_POINT('',(25.4466240721952,-5.74734553320186,-8.5));
#5966=CARTESIAN_POINT('Origin',(25.4466240721952,-8.04398219900198,-8.5));
#5967=CARTESIAN_POINT('',(25.4466240721952,-5.74734553320186,-6.5));
#5968=CARTESIAN_POINT('Origin',(25.4466240721952,-8.04398219900198,-6.5));
#5969=CARTESIAN_POINT('',(25.4466240721952,-5.74734553320186,-8.5));
#5970=CARTESIAN_POINT('Origin',(23.3121029357457,-5.74734553320186,-8.5));
#5971=CARTESIAN_POINT('',(23.3121029357457,-5.74734553320186,-8.5));
#5972=CARTESIAN_POINT('',(25.4466240721952,-5.74734553320186,-8.5));
#5973=CARTESIAN_POINT('',(23.3121029357457,-5.74734553320186,-6.5));
#5974=CARTESIAN_POINT('',(25.4466240721952,-5.74734553320186,-6.5));
#5975=CARTESIAN_POINT('',(23.3121029357457,-5.74734553320186,-8.5));
#5976=CARTESIAN_POINT('Origin',(23.3121029357457,-8.04398219900198,-8.5));
#5977=CARTESIAN_POINT('Origin',(23.3121029357457,-8.04398219900198,-8.5));
#5978=CARTESIAN_POINT('Origin',(23.3121029357457,-8.04398219900198,-6.5));
#5979=CARTESIAN_POINT('Origin',(19.2071026744088,-3.13165946910082,-8.5));
#5980=CARTESIAN_POINT('',(19.2071026744088,-9.4502026108178,-8.5));
#5981=CARTESIAN_POINT('',(19.2071026744088,-1.63165946910082,-8.5));
#5982=CARTESIAN_POINT('',(19.2071026744088,-9.4502026108178,-6.5));
#5983=CARTESIAN_POINT('',(19.2071026744088,-9.4502026108178,-8.5));
#5984=CARTESIAN_POINT('',(19.2071026744088,-9.4502026108178,-6.5));
#5985=CARTESIAN_POINT('Origin',(40.5218849555161,-9.45020261081779,-8.5));
#5986=CARTESIAN_POINT('',(40.5218849555161,-11.9502026108178,-8.5));
#5987=CARTESIAN_POINT('Origin',(40.5218849555161,-9.45020261081779,-8.5));
#5988=CARTESIAN_POINT('',(40.5218849555161,-11.9502026108178,-6.5));
#5989=CARTESIAN_POINT('Origin',(40.5218849555161,-9.45020261081779,-6.5));
#5990=CARTESIAN_POINT('',(40.5218849555161,-11.9502026108178,-8.5));
#5991=CARTESIAN_POINT('Origin',(21.7071026744088,-11.9502026108178,-8.5));
#5992=CARTESIAN_POINT('',(21.7071026744088,-11.9502026108178,-8.5));
#5993=CARTESIAN_POINT('',(40.5218849555161,-11.9502026108178,-8.5));
#5994=CARTESIAN_POINT('',(21.7071026744088,-11.9502026108178,-6.5));
#5995=CARTESIAN_POINT('',(40.5218849555161,-11.9502026108178,-6.5));
#5996=CARTESIAN_POINT('',(21.7071026744088,-11.9502026108178,-8.5));
#5997=CARTESIAN_POINT('Origin',(21.7071026744088,-9.4502026108178,-8.5));
#5998=CARTESIAN_POINT('Origin',(21.7071026744088,-9.4502026108178,-8.5));
#5999=CARTESIAN_POINT('Origin',(21.7071026744088,-9.4502026108178,-6.5));
#6000=CARTESIAN_POINT('Origin',(31.1144938149625,-7.54093103995931,-6.5));
#6001=CARTESIAN_POINT('Origin',(31.1144938149625,-7.54093103995931,-8.5));
#6002=CARTESIAN_POINT('',(0.,0.,0.));
#6003=CARTESIAN_POINT('Origin',(24.7143466872546,3.13165946910082,-0.395297377936459));
#6004=CARTESIAN_POINT('',(24.7143466872546,3.63165946910083,1.30603779103116));
#6005=CARTESIAN_POINT('Origin',(24.7143466872546,3.63165946910082,-0.395297377936459));
#6006=CARTESIAN_POINT('',(24.7143466872546,3.13165946910082,1.80603779103116));
#6007=CARTESIAN_POINT('Origin',(24.7143466872546,3.13165946910082,1.30603779103116));
#6008=CARTESIAN_POINT('Origin',(24.7143466872546,3.13165946910082,-0.395297377936459));
#6009=CARTESIAN_POINT('Origin',(24.7143466872546,3.63165946910082,-0.395297377936459));
#6010=CARTESIAN_POINT('Origin',(37.3390884548007,3.13165946910082,-0.451167579126729));
#6011=CARTESIAN_POINT('',(37.3390884548007,3.63165946910083,1.30858121201868));
#6012=CARTESIAN_POINT('Origin',(37.3390884548007,3.63165946910082,-0.451167579126729));
#6013=CARTESIAN_POINT('',(37.3390884548007,3.13165946910082,1.80858121201868));
#6014=CARTESIAN_POINT('Origin',(37.3390884548007,3.13165946910082,1.30858121201868));
#6015=CARTESIAN_POINT('Origin',(37.3390884548007,3.13165946910082,-0.451167579126729));
#6016=CARTESIAN_POINT('Origin',(37.3390884548007,3.63165946910082,-0.451167579126729));
#6017=CARTESIAN_POINT('Origin',(25.1607982446856,4.63165946910082,-5.));
#6018=CARTESIAN_POINT('',(19.2071026744088,4.63165946910082,-6.5));
#6019=CARTESIAN_POINT('',(19.8239560216472,3.13165946910082,-5.));
#6020=CARTESIAN_POINT('Origin',(19.8239560216472,4.63165946910082,-5.));
#6021=CARTESIAN_POINT('',(42.4050316082777,3.13165946910082,-5.));
#6022=CARTESIAN_POINT('',(25.1607982446856,3.13165946910082,-5.));
#6023=CARTESIAN_POINT('',(43.0218849555161,4.63165946910082,-6.5));
#6024=CARTESIAN_POINT('Origin',(42.4050316082777,4.63165946910082,-5.));
#6025=CARTESIAN_POINT('',(25.1607982446856,4.63165946910082,-6.5));
#6026=CARTESIAN_POINT('Origin',(31.1144938149625,7.54093103995931,-6.5));
#6027=CARTESIAN_POINT('',(43.0218849555161,9.4502026108178,-6.5));
#6028=CARTESIAN_POINT('',(43.0218849555161,3.13165946910082,-6.5));
#6029=CARTESIAN_POINT('',(40.5218849555161,11.9502026108178,-6.5));
#6030=CARTESIAN_POINT('Origin',(40.5218849555161,9.45020261081779,-6.5));
#6031=CARTESIAN_POINT('',(21.7071026744088,11.9502026108178,-6.5));
#6032=CARTESIAN_POINT('',(40.5218849555161,11.9502026108178,-6.5));
#6033=CARTESIAN_POINT('',(19.2071026744088,9.4502026108178,-6.5));
#6034=CARTESIAN_POINT('Origin',(21.7071026744088,9.4502026108178,-6.5));
#6035=CARTESIAN_POINT('',(19.2071026744088,9.4502026108178,-6.5));
#6036=CARTESIAN_POINT('',(36.8121029357457,10.3406188648021,-6.5));
#6037=CARTESIAN_POINT('',(36.8121029357457,5.74734553320186,-6.5));
#6038=CARTESIAN_POINT('Origin',(36.8121029357457,8.04398219900198,-6.5));
#6039=CARTESIAN_POINT('',(38.9466240721952,10.3406188648021,-6.5));
#6040=CARTESIAN_POINT('',(36.8121029357457,10.3406188648021,-6.5));
#6041=CARTESIAN_POINT('',(38.9466240721952,5.74734553320186,-6.5));
#6042=CARTESIAN_POINT('Origin',(38.9466240721952,8.04398219900198,-6.5));
#6043=CARTESIAN_POINT('',(38.9466240721952,5.74734553320186,-6.5));
#6044=CARTESIAN_POINT('',(23.3121029357457,10.3406188648021,-6.5));
#6045=CARTESIAN_POINT('',(23.3121029357457,5.74734553320186,-6.5));
#6046=CARTESIAN_POINT('Origin',(23.3121029357457,8.04398219900198,-6.5));
#6047=CARTESIAN_POINT('',(25.4466240721952,10.3406188648021,-6.5));
#6048=CARTESIAN_POINT('',(23.3121029357457,10.3406188648021,-6.5));
#6049=CARTESIAN_POINT('',(25.4466240721952,5.74734553320186,-6.5));
#6050=CARTESIAN_POINT('Origin',(25.4466240721952,8.04398219900198,-6.5));
#6051=CARTESIAN_POINT('',(25.4466240721952,5.74734553320186,-6.5));
#6052=CARTESIAN_POINT('Origin',(37.2590007645168,2.75665946910082,0.));
#6053=CARTESIAN_POINT('',(34.7590007645168,3.13165946910082,0.));
#6054=CARTESIAN_POINT('',(37.2590007645168,3.13165946910082,2.5));
#6055=CARTESIAN_POINT('Origin',(37.2590007645168,3.13165946910082,0.));
#6056=CARTESIAN_POINT('',(34.7590007645168,1.63165946910082,0.));
#6057=CARTESIAN_POINT('',(34.7590007645168,2.75665946910082,0.));
#6058=CARTESIAN_POINT('',(37.2590007645168,1.63165946910082,2.5));
#6059=CARTESIAN_POINT('Origin',(37.2590007645168,1.63165946910082,0.));
#6060=CARTESIAN_POINT('',(37.2590007645168,2.75665946910082,2.5));
#6061=CARTESIAN_POINT('Origin',(31.1144938149625,2.38165946910082,2.5));
#6062=CARTESIAN_POINT('',(37.4782084817555,1.63165946910082,2.5));
#6063=CARTESIAN_POINT('',(43.0218849555161,1.63165946910082,2.5));
#6064=CARTESIAN_POINT('',(37.4782084817555,3.13165946910082,2.5));
#6065=CARTESIAN_POINT('',(37.4782084817555,2.75665946910082,2.5));
#6066=CARTESIAN_POINT('',(19.2071026744088,3.13165946910082,2.5));
#6067=CARTESIAN_POINT('Origin',(19.2071026744088,3.13165946910082,-8.5));
#6068=CARTESIAN_POINT('',(22.2074408259328,3.13165946910082,0.795911171487552));
#6069=CARTESIAN_POINT('',(20.7059131671521,3.13165946910082,-2.85534807555141));
#6070=CARTESIAN_POINT('',(24.7507791481694,3.13165946910082,2.5));
#6071=CARTESIAN_POINT('Origin',(24.7507791481694,3.13165946910082,-0.25));
#6072=CARTESIAN_POINT('',(24.9699868654081,3.13165946910082,2.5));
#6073=CARTESIAN_POINT('',(19.2071026744088,3.13165946910082,2.5));
#6074=CARTESIAN_POINT('',(27.4699868654081,3.13165946910082,0.));
#6075=CARTESIAN_POINT('Origin',(24.9699868654081,3.13165946910082,0.));
#6076=CARTESIAN_POINT('',(27.4699868654081,3.13165946910082,-0.758936728277321));
#6077=CARTESIAN_POINT('',(27.4699868654081,3.13165946910082,-4.62946836413866));
#6078=CARTESIAN_POINT('',(27.5384895461752,3.13165946910082,-1.277895402736));
#6079=CARTESIAN_POINT('Origin',(29.4699868654084,3.13165946910082,-0.758936728277284));
#6080=CARTESIAN_POINT('',(34.6904980837498,3.13165946910082,-1.277895402736));
#6081=CARTESIAN_POINT('Origin',(31.1144938149625,3.13165946910082,-0.317087216926334));
#6082=CARTESIAN_POINT('',(34.7590007645168,3.13165946910082,-0.758936728277321));
#6083=CARTESIAN_POINT('Origin',(32.7590007645165,3.13165946910082,-0.758936728277284));
#6084=CARTESIAN_POINT('',(34.7590007645168,3.13165946910082,-3.));
#6085=CARTESIAN_POINT('',(40.0215468039921,3.13165946910082,0.79591117148755));
#6086=CARTESIAN_POINT('Origin',(37.4782084817555,3.13165946910082,-0.25));
#6087=CARTESIAN_POINT('',(41.6512074608448,3.13165946910082,-3.16692861243009));
#6088=CARTESIAN_POINT('Origin',(24.9699868654081,2.75665946910082,0.));
#6089=CARTESIAN_POINT('',(27.4699868654081,1.63165946910082,0.));
#6090=CARTESIAN_POINT('',(24.9699868654081,1.63165946910082,2.5));
#6091=CARTESIAN_POINT('Origin',(24.9699868654081,1.63165946910082,0.));
#6092=CARTESIAN_POINT('',(27.4699868654081,2.75665946910082,0.));
#6093=CARTESIAN_POINT('',(24.9699868654081,2.75665946910082,2.5));
#6094=CARTESIAN_POINT('Origin',(27.4699868654081,3.13165946910082,-0.758936728277321));
#6095=CARTESIAN_POINT('',(27.4699868654081,1.63165946910082,-0.758936728277321));
#6096=CARTESIAN_POINT('',(27.4699868654081,1.63165946910082,-4.62946836413866));
#6097=CARTESIAN_POINT('',(27.4699868654081,3.13165946910082,-0.758936728277321));
#6098=CARTESIAN_POINT('Origin',(37.4782084817555,2.75665946910082,-0.25));
#6099=CARTESIAN_POINT('',(40.0215468039921,1.63165946910082,0.795911171487551));
#6100=CARTESIAN_POINT('Origin',(37.4782084817555,1.63165946910082,-0.25));
#6101=CARTESIAN_POINT('',(40.0215468039921,2.75665946910082,0.795911171487553));
#6102=CARTESIAN_POINT('Origin',(43.0218849555161,3.13165946910082,-6.5));
#6103=CARTESIAN_POINT('',(43.0218849555161,1.63165946910082,-6.5));
#6104=CARTESIAN_POINT('',(43.373634504488,1.63165946910082,-7.35534807555141));
#6105=CARTESIAN_POINT('',(43.0218849555161,3.13165946910082,-6.5));
#6106=CARTESIAN_POINT('Origin',(24.7507791481694,2.75665946910082,-0.25));
#6107=CARTESIAN_POINT('',(22.2074408259328,1.63165946910082,0.795911171487552));
#6108=CARTESIAN_POINT('',(22.2074408259328,2.75665946910082,0.795911171487551));
#6109=CARTESIAN_POINT('',(24.7507791481694,1.63165946910082,2.5));
#6110=CARTESIAN_POINT('Origin',(24.7507791481694,1.63165946910082,-0.25));
#6111=CARTESIAN_POINT('',(24.7507791481694,2.75665946910082,2.5));
#6112=CARTESIAN_POINT('Origin',(22.9082227578391,3.13165946910082,2.5));
#6113=CARTESIAN_POINT('',(19.2071026744088,1.63165946910082,-6.5));
#6114=CARTESIAN_POINT('',(19.2071026744088,3.13165946910083,-6.5));
#6115=CARTESIAN_POINT('',(22.4283402107953,1.63165946910082,1.3330713875699));
#6116=CARTESIAN_POINT('Origin',(32.7590007645165,3.13165946910082,-0.758936728277284));
#6117=CARTESIAN_POINT('',(34.6904980837498,1.63165946910082,-1.277895402736));
#6118=CARTESIAN_POINT('',(34.7590007645168,1.63165946910082,-0.758936728277321));
#6119=CARTESIAN_POINT('Origin',(32.7590007645165,1.63165946910082,-0.758936728277284));
#6120=CARTESIAN_POINT('',(34.7590007645168,3.13165946910082,-0.758936728277321));
#6121=CARTESIAN_POINT('',(34.6904980837498,3.13165946910082,-1.277895402736));
#6122=CARTESIAN_POINT('Origin',(34.7590007645168,3.13165946910082,2.5));
#6123=CARTESIAN_POINT('',(34.7590007645168,1.63165946910082,-3.));
#6124=CARTESIAN_POINT('Origin',(29.4699868654084,3.13165946910082,-0.758936728277284));
#6125=CARTESIAN_POINT('',(27.5384895461752,1.63165946910082,-1.277895402736));
#6126=CARTESIAN_POINT('Origin',(29.4699868654084,1.63165946910082,-0.758936728277284));
#6127=CARTESIAN_POINT('',(27.5384895461752,3.13165946910082,-1.277895402736));
#6128=CARTESIAN_POINT('Origin',(31.1144938149625,3.13165946910082,-0.317087216926334));
#6129=CARTESIAN_POINT('Origin',(31.1144938149625,1.63165946910082,-0.317087216926334));
#6130=CARTESIAN_POINT('Origin',(43.0218849555161,9.4502026108178,-8.5));
#6131=CARTESIAN_POINT('',(43.0218849555161,1.63165946910082,-8.5));
#6132=CARTESIAN_POINT('',(43.0218849555161,1.63165946910082,-8.5));
#6133=CARTESIAN_POINT('',(43.0218849555161,9.4502026108178,-8.5));
#6134=CARTESIAN_POINT('',(43.0218849555161,3.13165946910082,-8.5));
#6135=CARTESIAN_POINT('',(43.0218849555161,9.4502026108178,-8.5));
#6136=CARTESIAN_POINT('Origin',(43.0218849555161,1.63165946910082,-8.5));
#6137=CARTESIAN_POINT('',(43.0218849555161,1.63165946910082,2.5));
#6138=CARTESIAN_POINT('',(19.2071026744088,1.63165946910082,-8.5));
#6139=CARTESIAN_POINT('',(19.2071026744088,1.63165946910082,-8.5));
#6140=CARTESIAN_POINT('',(43.0218849555161,1.63165946910082,-8.5));
#6141=CARTESIAN_POINT('Origin',(31.1144938149625,2.38165946910082,2.5));
#6142=CARTESIAN_POINT('Origin',(38.9466240721952,10.3406188648021,-8.5));
#6143=CARTESIAN_POINT('',(38.9466240721952,10.3406188648021,-8.5));
#6144=CARTESIAN_POINT('',(36.8121029357457,10.3406188648021,-8.5));
#6145=CARTESIAN_POINT('',(36.8121029357457,10.3406188648021,-8.5));
#6146=CARTESIAN_POINT('',(38.9466240721952,10.3406188648021,-8.5));
#6147=CARTESIAN_POINT('',(36.8121029357457,10.3406188648021,-8.5));
#6148=CARTESIAN_POINT('Origin',(38.9466240721952,8.04398219900198,-8.5));
#6149=CARTESIAN_POINT('',(38.9466240721952,5.74734553320186,-8.5));
#6150=CARTESIAN_POINT('Origin',(38.9466240721952,8.04398219900198,-8.5));
#6151=CARTESIAN_POINT('',(38.9466240721952,5.74734553320186,-8.5));
#6152=CARTESIAN_POINT('Origin',(36.8121029357457,5.74734553320186,-8.5));
#6153=CARTESIAN_POINT('',(36.8121029357457,5.74734553320186,-8.5));
#6154=CARTESIAN_POINT('',(38.9466240721952,5.74734553320186,-8.5));
#6155=CARTESIAN_POINT('',(36.8121029357457,5.74734553320186,-8.5));
#6156=CARTESIAN_POINT('Origin',(36.8121029357457,8.04398219900198,-8.5));
#6157=CARTESIAN_POINT('Origin',(36.8121029357457,8.04398219900198,-8.5));
#6158=CARTESIAN_POINT('Origin',(25.4466240721952,10.3406188648021,-8.5));
#6159=CARTESIAN_POINT('',(25.4466240721952,10.3406188648021,-8.5));
#6160=CARTESIAN_POINT('',(23.3121029357457,10.3406188648021,-8.5));
#6161=CARTESIAN_POINT('',(23.3121029357457,10.3406188648021,-8.5));
#6162=CARTESIAN_POINT('',(25.4466240721952,10.3406188648021,-8.5));
#6163=CARTESIAN_POINT('',(23.3121029357457,10.3406188648021,-8.5));
#6164=CARTESIAN_POINT('Origin',(25.4466240721952,8.04398219900198,-8.5));
#6165=CARTESIAN_POINT('',(25.4466240721952,5.74734553320186,-8.5));
#6166=CARTESIAN_POINT('Origin',(25.4466240721952,8.04398219900198,-8.5));
#6167=CARTESIAN_POINT('',(25.4466240721952,5.74734553320186,-8.5));
#6168=CARTESIAN_POINT('Origin',(23.3121029357457,5.74734553320186,-8.5));
#6169=CARTESIAN_POINT('',(23.3121029357457,5.74734553320186,-8.5));
#6170=CARTESIAN_POINT('',(25.4466240721952,5.74734553320186,-8.5));
#6171=CARTESIAN_POINT('',(23.3121029357457,5.74734553320186,-8.5));
#6172=CARTESIAN_POINT('Origin',(23.3121029357457,8.04398219900198,-8.5));
#6173=CARTESIAN_POINT('Origin',(23.3121029357457,8.04398219900198,-8.5));
#6174=CARTESIAN_POINT('Origin',(19.2071026744088,3.13165946910082,-8.5));
#6175=CARTESIAN_POINT('',(19.2071026744088,9.4502026108178,-8.5));
#6176=CARTESIAN_POINT('',(19.2071026744088,9.4502026108178,-8.5));
#6177=CARTESIAN_POINT('',(19.2071026744088,1.63165946910082,-8.5));
#6178=CARTESIAN_POINT('Origin',(40.5218849555161,9.45020261081779,-8.5));
#6179=CARTESIAN_POINT('',(40.5218849555161,11.9502026108178,-8.5));
#6180=CARTESIAN_POINT('Origin',(40.5218849555161,9.45020261081779,-8.5));
#6181=CARTESIAN_POINT('',(40.5218849555161,11.9502026108178,-8.5));
#6182=CARTESIAN_POINT('Origin',(21.7071026744088,11.9502026108178,-8.5));
#6183=CARTESIAN_POINT('',(21.7071026744088,11.9502026108178,-8.5));
#6184=CARTESIAN_POINT('',(40.5218849555161,11.9502026108178,-8.5));
#6185=CARTESIAN_POINT('',(21.7071026744088,11.9502026108178,-8.5));
#6186=CARTESIAN_POINT('Origin',(21.7071026744088,9.4502026108178,-8.5));
#6187=CARTESIAN_POINT('Origin',(21.7071026744088,9.4502026108178,-8.5));
#6188=CARTESIAN_POINT('Origin',(31.1144938149625,7.54093103995931,-8.5));
#6189=CARTESIAN_POINT('',(0.,0.,0.));
#6190=CARTESIAN_POINT('Origin',(5.09382715545311,0.,8.60636253116605));
#6191=CARTESIAN_POINT('',(7.59382715545311,3.06161699786838E-16,8.60636253116605));
#6192=CARTESIAN_POINT('Origin',(5.09382715545311,0.,8.60636253116605));
#6193=CARTESIAN_POINT('',(7.59382715545311,3.06161699786838E-16,5.60636253116605));
#6194=CARTESIAN_POINT('',(7.59382715545311,-3.06161699786838E-16,8.60636253116605));
#6195=CARTESIAN_POINT('Origin',(5.09382715545311,0.,5.60636253116605));
#6196=CARTESIAN_POINT('Origin',(9.71262930897012,-1.11022302462516E-15,
8.60636253116605));
#6197=CARTESIAN_POINT('',(7.40322823221161,-4.,8.60636253116605));
#6198=CARTESIAN_POINT('',(9.71262930897012,-1.11022302462516E-15,8.60636253116605));
#6199=CARTESIAN_POINT('',(7.40322823221161,-4.,8.60636253116605));
#6200=CARTESIAN_POINT('',(7.40322823221161,-4.,5.60636253116605));
#6201=CARTESIAN_POINT('',(7.40322823221161,-4.,8.60636253116605));
#6202=CARTESIAN_POINT('',(9.71262930897012,-1.11022302462516E-15,5.60636253116605));
#6203=CARTESIAN_POINT('',(7.40322823221161,-4.,5.60636253116605));
#6204=CARTESIAN_POINT('',(9.71262930897012,-1.11022302462516E-15,8.60636253116605));
#6205=CARTESIAN_POINT('Origin',(7.40322823221161,4.,8.60636253116605));
#6206=CARTESIAN_POINT('',(7.40322823221161,4.,8.60636253116605));
#6207=CARTESIAN_POINT('',(9.71262930897012,-1.11022302462516E-15,8.60636253116605));
#6208=CARTESIAN_POINT('',(7.40322823221161,4.,5.60636253116605));
#6209=CARTESIAN_POINT('',(9.71262930897012,-1.11022302462516E-15,5.60636253116605));
#6210=CARTESIAN_POINT('',(7.40322823221161,4.,8.60636253116605));
#6211=CARTESIAN_POINT('Origin',(2.78442607869461,4.,8.60636253116605));
#6212=CARTESIAN_POINT('',(2.78442607869461,4.,8.60636253116605));
#6213=CARTESIAN_POINT('',(7.40322823221161,4.,8.60636253116605));
#6214=CARTESIAN_POINT('',(2.78442607869461,4.,5.60636253116605));
#6215=CARTESIAN_POINT('',(7.40322823221161,4.,5.60636253116605));
#6216=CARTESIAN_POINT('',(2.78442607869461,4.,8.60636253116605));
#6217=CARTESIAN_POINT('Origin',(0.4750250019361,2.77555756156289E-15,8.60636253116605));
#6218=CARTESIAN_POINT('',(0.4750250019361,2.77555756156289E-15,8.60636253116605));
#6219=CARTESIAN_POINT('',(2.78442607869461,4.,8.60636253116605));
#6220=CARTESIAN_POINT('',(0.4750250019361,2.77555756156289E-15,5.60636253116605));
#6221=CARTESIAN_POINT('',(2.78442607869461,4.,5.60636253116605));
#6222=CARTESIAN_POINT('',(0.4750250019361,2.77555756156289E-15,8.60636253116605));
#6223=CARTESIAN_POINT('Origin',(2.7844260786946,-4.,8.60636253116605));
#6224=CARTESIAN_POINT('',(2.7844260786946,-4.,8.60636253116605));
#6225=CARTESIAN_POINT('',(0.4750250019361,2.77555756156289E-15,8.60636253116605));
#6226=CARTESIAN_POINT('',(2.7844260786946,-4.,5.60636253116605));
#6227=CARTESIAN_POINT('',(0.4750250019361,2.77555756156289E-15,5.60636253116605));
#6228=CARTESIAN_POINT('',(2.7844260786946,-4.,8.60636253116605));
#6229=CARTESIAN_POINT('Origin',(7.40322823221161,-4.,8.60636253116605));
#6230=CARTESIAN_POINT('',(2.7844260786946,-4.,8.60636253116605));
#6231=CARTESIAN_POINT('',(2.7844260786946,-4.,5.60636253116605));
#6232=CARTESIAN_POINT('Origin',(5.09382715545311,5.55111512312578E-16,8.60636253116605));
#6233=CARTESIAN_POINT('Origin',(5.09382715545311,5.55111512312578E-16,5.60636253116605));
#6234=CARTESIAN_POINT('',(0.,0.,0.));
#6235=CARTESIAN_POINT('Origin',(5.09382715545311,0.,-6.77268258743872));
#6236=CARTESIAN_POINT('',(7.08857715545311,-1.48167178722712E-8,-4.61281584510352));
#6237=CARTESIAN_POINT('',(7.08857671412439,-0.00132690645140175,-4.77268258743872));
#6238=CARTESIAN_POINT('',(7.08857715545311,8.3550772080578E-14,-6.77268258743872));
#6239=CARTESIAN_POINT('',(6.2322442180908,1.63799699450132,-5.29363746883395));
#6240=CARTESIAN_POINT('Ctrl Pts',(7.08857715545311,-1.48167178722712E-8,
-4.61281584510352));
#6241=CARTESIAN_POINT('Ctrl Pts',(7.08857715515529,-0.0400947307971134,
-4.61544918220441));
#6242=CARTESIAN_POINT('Ctrl Pts',(7.0873683003548,-0.0801825303907697,-4.61811867810323));
#6243=CARTESIAN_POINT('Ctrl Pts',(7.07727049993181,-0.247440799661336,-4.62940828682582));
#6244=CARTESIAN_POINT('Ctrl Pts',(7.05741240048877,-0.373631769826948,-4.6383184861514));
#6245=CARTESIAN_POINT('Ctrl Pts',(7.00135287300863,-0.591512757714937,-4.65398174107726));
#6246=CARTESIAN_POINT('Ctrl Pts',(6.97014883384365,-0.684078311974067,-4.66072168793572));
#6247=CARTESIAN_POINT('Ctrl Pts',(6.92804514054676,-0.784086582838243,-4.66785393707128));
#6248=CARTESIAN_POINT('Ctrl Pts',(6.92371465678162,-0.794140498682412,-4.66856912793543));
#6249=CARTESIAN_POINT('Ctrl Pts',(6.91703252460397,-0.80930922547275,-4.66964484456109));
#6250=CARTESIAN_POINT('Ctrl Pts',(6.9147417128135,-0.814450377374438,-4.67000885662465));
#6251=CARTESIAN_POINT('Ctrl Pts',(6.91058268033754,-0.823679016097091,-4.6706611388414));
#6252=CARTESIAN_POINT('Ctrl Pts',(6.90872238990846,-0.8277699244717,-4.67094987407352));
#6253=CARTESIAN_POINT('Ctrl Pts',(6.90460481660111,-0.836744145192207,-4.67158236707836));
#6254=CARTESIAN_POINT('Ctrl Pts',(6.90234160175738,-0.841624620463466,-4.67192575795504));
#6255=CARTESIAN_POINT('Ctrl Pts',(6.89577780104207,-0.855630291153922,-4.67290969774183));
#6256=CARTESIAN_POINT('Ctrl Pts',(6.89142762871411,-0.864732255025353,-4.67354729854128));
#6257=CARTESIAN_POINT('Ctrl Pts',(6.85946477911054,-0.930325201194365,-4.67813158667197));
#6258=CARTESIAN_POINT('Ctrl Pts',(6.82926078743822,-0.985521692584171,-4.68193274237631));
#6259=CARTESIAN_POINT('Ctrl Pts',(6.74901098783228,-1.11700580624151,-4.69106971997584));
#6260=CARTESIAN_POINT('Ctrl Pts',(6.69624707153906,-1.19146436221979,-4.6963199151433));
#6261=CARTESIAN_POINT('Ctrl Pts',(6.55742275297117,-1.36138427180224,-4.70907614350377));
#6262=CARTESIAN_POINT('Ctrl Pts',(6.46689259400708,-1.45264043881999,-4.71661590767991));
#6263=CARTESIAN_POINT('Ctrl Pts',(6.3557489127286,-1.54494160516324,-4.72557527884981));
#6264=CARTESIAN_POINT('Ctrl Pts',(6.34313466569004,-1.55515973634511,-4.72658781247032));
#6265=CARTESIAN_POINT('Ctrl Pts',(6.32237361935444,-1.57156155225421,-4.72824814092839));
#6266=CARTESIAN_POINT('Ctrl Pts',(6.31430134311785,-1.57783867283577,-4.72889222466277));
#6267=CARTESIAN_POINT('Ctrl Pts',(6.29978192139657,-1.58895110203977,-4.7300482784867));
#6268=CARTESIAN_POINT('Ctrl Pts',(6.29335302089738,-1.59380996270127,-4.73055931069375));
#6269=CARTESIAN_POINT('Ctrl Pts',(6.27966772771486,-1.60402338643849,-4.73164546739798));
#6270=CARTESIAN_POINT('Ctrl Pts',(6.27240413063881,-1.60936794930186,-4.73222096407933));
#6271=CARTESIAN_POINT('Ctrl Pts',(6.25287004646879,-1.62353798533996,-4.73376616418403));
#6272=CARTESIAN_POINT('Ctrl Pts',(6.24053526541135,-1.63227341546723,-4.73473928172537));
#6273=CARTESIAN_POINT('Ctrl Pts',(6.17826093377316,-1.67532152531414,-4.73964036149228));
#6274=CARTESIAN_POINT('Ctrl Pts',(6.12688017056799,-1.70748324017133,-4.74364771664052));
#6275=CARTESIAN_POINT('Ctrl Pts',(5.96291474065865,-1.80000515005531,-4.7563320750856));
#6276=CARTESIAN_POINT('Ctrl Pts',(5.84595120515671,-1.85192722898832,-4.76525737892825));
#6277=CARTESIAN_POINT('Ctrl Pts',(5.6328247064913,-1.92299730751201,-4.78089415862207));
#6278=CARTESIAN_POINT('Ctrl Pts',(5.53867674249202,-1.9469335538999,-4.78759396831812));
#6279=CARTESIAN_POINT('Ctrl Pts',(5.43235884025432,-1.96584435240037,-4.79469128894282));
#6280=CARTESIAN_POINT('Ctrl Pts',(5.42155068496735,-1.96767502922678,-4.7954074228328));
#6281=CARTESIAN_POINT('Ctrl Pts',(5.40515987895374,-1.97031248818372,-4.79648477745489));
#6282=CARTESIAN_POINT('Ctrl Pts',(5.39958820031319,-1.97118480897772,-4.79684948487212));
#6283=CARTESIAN_POINT('Ctrl Pts',(5.38955382730705,-1.97271225507761,-4.79750349341496));
#6284=CARTESIAN_POINT('Ctrl Pts',(5.38509258255286,-1.97337587848556,-4.79779325599492));
#6285=CARTESIAN_POINT('Ctrl Pts',(5.37527424371394,-1.9748023641512,-4.79842876016531));
#6286=CARTESIAN_POINT('Ctrl Pts',(5.36991628869129,-1.97555856230869,-4.79877412811315));
#6287=CARTESIAN_POINT('Ctrl Pts',(5.3544878673316,-1.97767206833307,-4.79976467899655));
#6288=CARTESIAN_POINT('Ctrl Pts',(5.34440984664975,-1.97897426503916,-4.80040688279367));
#6289=CARTESIAN_POINT('Ctrl Pts',(5.27067772117271,-1.98792902018792,-4.80507290662605));
#6290=CARTESIAN_POINT('Ctrl Pts',(5.20669059594675,-1.99258664349983,-4.80894626086477));
#6291=CARTESIAN_POINT('Ctrl Pts',(5.00659272338178,-1.99747900392144,-4.82081444578765));
#6292=CARTESIAN_POINT('Ctrl Pts',(4.87061587215657,-1.9868849133802,-4.82855057247952));
#6293=CARTESIAN_POINT('Ctrl Pts',(4.65604088092438,-1.94784595316983,-4.84142773341889));
#6294=CARTESIAN_POINT('Ctrl Pts',(4.57630245148535,-1.92819255035695,-4.84636193642796));
#6295=CARTESIAN_POINT('Ctrl Pts',(4.48329474201247,-1.89908277104335,-4.85241289230236));
#6296=CARTESIAN_POINT('Ctrl Pts',(4.46863721086776,-1.89430797697619,-4.85337527953983));
#6297=CARTESIAN_POINT('Ctrl Pts',(4.4445753087319,-1.88615995797207,-4.85497037589027));
#6298=CARTESIAN_POINT('Ctrl Pts',(4.4351381533715,-1.88288505763404,-4.85559987359212));
#6299=CARTESIAN_POINT('Ctrl Pts',(4.41813803594403,-1.87684219652712,-4.85674108532922));
#6300=CARTESIAN_POINT('Ctrl Pts',(4.41056643845231,-1.87409903857928,-4.85725197343053));
#6301=CARTESIAN_POINT('Ctrl Pts',(4.39437370686075,-1.86812130766766,-4.85835026905944));
#6302=CARTESIAN_POINT('Ctrl Pts',(4.38575796957072,-1.86487274907785,-4.85893813033501));
#6303=CARTESIAN_POINT('Ctrl Pts',(4.36230536462303,-1.85584400518734,-4.8605480280963));
#6304=CARTESIAN_POINT('Ctrl Pts',(4.34751497817963,-1.84994573213895,-4.86157397246172));
#6305=CARTESIAN_POINT('Ctrl Pts',(4.26604076303032,-1.81631847830108,-4.86728609052941));
#6306=CARTESIAN_POINT('Ctrl Pts',(4.20083769700026,-1.78516408602775,-4.87208670876007));
#6307=CARTESIAN_POINT('Ctrl Pts',(4.00824617895935,-1.6799480055716,-4.88697874456887));
#6308=CARTESIAN_POINT('Ctrl Pts',(3.88723954816717,-1.59525872597823,-4.89737444923679));
#6309=CARTESIAN_POINT('Ctrl Pts',(3.76106781248094,-1.4843219981909,-4.90896301151816));
#6310=CARTESIAN_POINT('Ctrl Pts',(3.74567909414366,-1.47035917679528,-4.91038982975238));
#6311=CARTESIAN_POINT('Ctrl Pts',(3.69672988504033,-1.42453087882556,-4.91496537723626));
#6312=CARTESIAN_POINT('Ctrl Pts',(3.66405652730914,-1.39173478381734,-4.91807751757299));
#6313=CARTESIAN_POINT('Ctrl Pts',(3.62652904699974,-1.35134824842086,-4.9216925637817));
#6314=CARTESIAN_POINT('Ctrl Pts',(3.62055009565997,-1.34482732703748,-4.92226980080627));
#6315=CARTESIAN_POINT('Ctrl Pts',(3.61083639125473,-1.33409057812522,-4.92320940507348));
#6316=CARTESIAN_POINT('Ctrl Pts',(3.60707583263341,-1.32989841089904,-4.92357361086162));
#6317=CARTESIAN_POINT('Ctrl Pts',(3.60035354389009,-1.32234043764107,-4.92422537471545));
#6318=CARTESIAN_POINT('Ctrl Pts',(3.597385341909,-1.3189805008644,-4.92451340917361));
#6319=CARTESIAN_POINT('Ctrl Pts',(3.5909086290735,-1.31159900364749,-4.92514243459031));
#6320=CARTESIAN_POINT('Ctrl Pts',(3.58740491633508,-1.30757335641467,-4.92548307230828));
#6321=CARTESIAN_POINT('Ctrl Pts',(3.57737584996034,-1.29595648272935,-4.92645930351697));
#6322=CARTESIAN_POINT('Ctrl Pts',(3.57089131441462,-1.28833000472427,-4.92709196714809));
#6323=CARTESIAN_POINT('Ctrl Pts',(3.52448166516577,-1.23290742648859,-4.93163328279849));
#6324=CARTESIAN_POINT('Ctrl Pts',(3.48675254618516,-1.18330844017394,-4.93539778804676));
#6325=CARTESIAN_POINT('Ctrl Pts',(3.39919089019986,-1.05626705578178,-4.9445465152989));
#6326=CARTESIAN_POINT('Ctrl Pts',(3.35228026933408,-0.97698931312293,-4.94983891668592));
#6327=CARTESIAN_POINT('Ctrl Pts',(3.25311619480361,-0.779402390041069,-4.96267537833802));
#6328=CARTESIAN_POINT('Ctrl Pts',(3.20656356209051,-0.658721982534789,-4.97025327754844));
#6329=CARTESIAN_POINT('Ctrl Pts',(3.16766022697015,-0.518816124761333,-4.97925591514562));
#6330=CARTESIAN_POINT('Ctrl Pts',(3.16351659099316,-0.503180194681899,-4.98026456673374));
#6331=CARTESIAN_POINT('Ctrl Pts',(3.15707891071831,-0.477637069939258,-4.98191719976237));
#6332=CARTESIAN_POINT('Ctrl Pts',(3.15466960846471,-0.467759485037016,-4.98255745585297));
#6333=CARTESIAN_POINT('Ctrl Pts',(3.15050021851563,-0.450079927691032,-4.98370571725798));
#6334=CARTESIAN_POINT('Ctrl Pts',(3.14871133108398,-0.442284921596935,-4.98421278243635));
#6335=CARTESIAN_POINT('Ctrl Pts',(3.14502351138985,-0.425760180928002,-4.98528948308725));
#6336=CARTESIAN_POINT('Ctrl Pts',(3.14313625776749,-0.41702804721845,-4.98585948152347));
#6337=CARTESIAN_POINT('Ctrl Pts',(3.13825134764445,-0.393667126727878,-4.9873873057125));
#6338=CARTESIAN_POINT('Ctrl Pts',(3.1353592409189,-0.379017089723568,-4.98834848135653));
#6339=CARTESIAN_POINT('Ctrl Pts',(3.12182138282397,-0.306143804023358,-4.993145722628));
#6340=CARTESIAN_POINT('Ctrl Pts',(3.11360720870425,-0.24750464213578,-4.99705805834837));
#6341=CARTESIAN_POINT('Ctrl Pts',(3.09701745954933,-0.0728196042003857,
-5.00887189309357));
#6342=CARTESIAN_POINT('Ctrl Pts',(3.09616900309937,0.0436810129057251,-5.01697136695062));
#6343=CARTESIAN_POINT('Ctrl Pts',(3.11363990879115,0.261370512183108,-5.03220192407051));
#6344=CARTESIAN_POINT('Ctrl Pts',(3.12961504059217,0.362396192732447,-5.03930375089956));
#6345=CARTESIAN_POINT('Ctrl Pts',(3.15703518181583,0.477630041467434,-5.0471582693509));
#6346=CARTESIAN_POINT('Ctrl Pts',(3.16100558520107,0.493451541969581,-5.04823098521159));
#6347=CARTESIAN_POINT('Ctrl Pts',(3.16687847548655,0.515694821989584,-5.04972933867866));
#6348=CARTESIAN_POINT('Ctrl Pts',(3.1686197812671,0.522157959002024,-5.05016353886671));
#6349=CARTESIAN_POINT('Ctrl Pts',(3.17160784005498,0.533030449615308,-5.05089184696418));
#6350=CARTESIAN_POINT('Ctrl Pts',(3.17283730196313,0.537444454071113,-5.05118693353936));
#6351=CARTESIAN_POINT('Ctrl Pts',(3.1753914786931,0.546493692024882,-5.05179063611881));
#6352=CARTESIAN_POINT('Ctrl Pts',(3.17671779487256,0.5511283898126,-5.05209915913269));
#6353=CARTESIAN_POINT('Ctrl Pts',(3.18015521981358,0.562977610470331,-5.05288632485509));
#6354=CARTESIAN_POINT('Ctrl Pts',(3.18229035364499,0.570185168845214,-5.05336360109104));
#6355=CARTESIAN_POINT('Ctrl Pts',(3.19126970718108,0.599879318977058,-5.05532422318489));
#6356=CARTESIAN_POINT('Ctrl Pts',(3.19847068057325,0.622257172053322,-5.0567882694558));
#6357=CARTESIAN_POINT('Ctrl Pts',(3.21874071946015,0.681628433729931,-5.06064926655386));
#6358=CARTESIAN_POINT('Ctrl Pts',(3.23250874331918,0.718373587059294,-5.06301445747872));
#6359=CARTESIAN_POINT('Ctrl Pts',(3.28324289446776,0.842502992402395,-5.07099527907893));
#6360=CARTESIAN_POINT('Ctrl Pts',(3.32535350892617,0.927647251040959,-5.07645855214757));
#6361=CARTESIAN_POINT('Ctrl Pts',(3.43959101262252,1.12234378590508,-5.08957745425663));
#6362=CARTESIAN_POINT('Ctrl Pts',(3.51675249593857,1.22840620137394,-5.09726287174244));
#6363=CARTESIAN_POINT('Ctrl Pts',(3.61456781561203,1.33831417118987,-5.10638892053515));
#6364=CARTESIAN_POINT('Ctrl Pts',(3.62554794010361,1.35035148636723,-5.10740536135711));
#6365=CARTESIAN_POINT('Ctrl Pts',(3.64368682446066,1.36975400418078,-5.10907245717445));
#6366=CARTESIAN_POINT('Ctrl Pts',(3.65075732207012,1.37720095165135,-5.10971939058417));
#6367=CARTESIAN_POINT('Ctrl Pts',(3.66350469653888,1.39042107874366,-5.11088079550017));
#6368=CARTESIAN_POINT('Ctrl Pts',(3.66915985602239,1.39621495318322,-5.11139432659713));
#6369=CARTESIAN_POINT('Ctrl Pts',(3.68122094243299,1.4084223145352,-5.11248606560021));
#6370=CARTESIAN_POINT('Ctrl Pts',(3.68763561171649,1.41482686821925,-5.11306464907469));
#6371=CARTESIAN_POINT('Ctrl Pts',(3.70492603614829,1.43185628105505,-5.11461887322415));
#6372=CARTESIAN_POINT('Ctrl Pts',(3.71587981704447,1.4424007211425,-5.11559795270281));
#6373=CARTESIAN_POINT('Ctrl Pts',(3.77152328685271,1.49475249209425,-5.12054497786874));
#6374=CARTESIAN_POINT('Ctrl Pts',(3.81799544058498,1.53460895886861,-5.12459343596775));
#6375=CARTESIAN_POINT('Ctrl Pts',(3.96908172653465,1.65257539009432,-5.13751048811448));
#6376=CARTESIAN_POINT('Ctrl Pts',(4.07956606839761,1.72259260882287,-5.1466369508837));
#6377=CARTESIAN_POINT('Ctrl Pts',(4.27857703879079,1.82289041387427,-5.16212226696692));
#6378=CARTESIAN_POINT('Ctrl Pts',(4.36387414234001,1.8586916851381,-5.16848442723695));
#6379=CARTESIAN_POINT('Ctrl Pts',(4.46166116029799,1.89195989236394,-5.17527070293879));
#6380=CARTESIAN_POINT('Ctrl Pts',(4.47199640601663,1.89538191702214,-5.17598174371719));
#6381=CARTESIAN_POINT('Ctrl Pts',(4.48769219062187,1.90043662213043,-5.17705165927343));
#6382=CARTESIAN_POINT('Ctrl Pts',(4.49303225058894,1.9021315502465,-5.1774139392048));
#6383=CARTESIAN_POINT('Ctrl Pts',(4.50266930301365,1.90514570544937,-5.17806453420173));
#6384=CARTESIAN_POINT('Ctrl Pts',(4.5069635931026,1.90647290175745,-5.17835329019095));
#6385=CARTESIAN_POINT('Ctrl Pts',(4.51130368123066,1.90779819853609,-5.17864398511427));
#6386=CARTESIAN_POINT('Ctrl Pts',(4.51134490418714,1.90781078498836,-5.17864674608481));
#6387=CARTESIAN_POINT('Ctrl Pts',(4.51142619629517,1.90783560272552,-5.1786521905442));
#6388=CARTESIAN_POINT('Ctrl Pts',(4.51146626542467,1.90784783408437,-5.17865487403729));
#6389=CARTESIAN_POINT('Ctrl Pts',(4.51154529592963,1.90787195593133,-5.17866016664289));
#6390=CARTESIAN_POINT('Ctrl Pts',(4.51158425730295,1.90788384649409,-5.17866277576058));
#6391=CARTESIAN_POINT('Ctrl Pts',(4.51166111600311,1.90790730031126,-5.17866792255817));
#6392=CARTESIAN_POINT('Ctrl Pts',(4.51169901329897,1.90791886362657,-5.17867046024098));
#6393=CARTESIAN_POINT('Ctrl Pts',(4.51177378521746,1.90794167578141,-5.17867546695405));
#6394=CARTESIAN_POINT('Ctrl Pts',(4.51181065982405,1.90795292468183,-5.1786779359879));
#6395=CARTESIAN_POINT('Ctrl Pts',(4.51188342566564,1.90797512019131,-5.17868280804843));
#6396=CARTESIAN_POINT('Ctrl Pts',(4.51191931687129,1.90798606685296,-5.17868521107751));
#6397=CARTESIAN_POINT('Ctrl Pts',(4.51199015315827,1.90800766942779,-5.17868995363527));
#6398=CARTESIAN_POINT('Ctrl Pts',(4.51202509823475,1.90801832539711,-5.1786922931677));
#6399=CARTESIAN_POINT('Ctrl Pts',(4.51209407772082,1.90803935757052,-5.17869691111814));
#6400=CARTESIAN_POINT('Ctrl Pts',(4.51212811210257,1.90804973382013,-5.1786991895381));
#6401=CARTESIAN_POINT('Ctrl Pts',(4.51219530386416,1.90807021697808,-5.17870368752863));
#6402=CARTESIAN_POINT('Ctrl Pts',(4.51222846122625,1.90808032393167,-5.1787059071016));
#6403=CARTESIAN_POINT('Ctrl Pts',(4.51229393094737,1.9081002784018,-5.17871028955084));
#6404=CARTESIAN_POINT('Ctrl Pts',(4.51232624330227,1.90811012596464,-5.17871245243019));
#6405=CARTESIAN_POINT('Ctrl Pts',(4.51239005356905,1.90812957110803,-5.17871672354777));
#6406=CARTESIAN_POINT('Ctrl Pts',(4.51242155143479,1.90813916871918,-5.17871883178607));
#6407=CARTESIAN_POINT('Ctrl Pts',(4.5124837616893,1.90815812291801,-5.17872299556973));
#6408=CARTESIAN_POINT('Ctrl Pts',(4.51251447408323,1.90816747954926,-5.17872505111839));
#6409=CARTESIAN_POINT('Ctrl Pts',(4.5125751410553,1.90818596034009,-5.17872911138295));
#6410=CARTESIAN_POINT('Ctrl Pts',(4.51260509563796,1.90819508454056,-5.17873111610192));
#6411=CARTESIAN_POINT('Ctrl Pts',(4.51266427340371,1.90821310863363,-5.17873507648332));
#6412=CARTESIAN_POINT('Ctrl Pts',(4.51269349656876,1.90822200855794,-5.17873703214715));
#6413=CARTESIAN_POINT('Ctrl Pts',(4.51275123664262,1.90823959186659,-5.17874089610871));
#6414=CARTESIAN_POINT('Ctrl Pts',(4.51277975355018,1.9082482752856,-5.17874280440882));
#6415=CARTESIAN_POINT('Ctrl Pts',(4.51814791843944,1.90988275389405,-5.17910202306494));
#6416=CARTESIAN_POINT('Ctrl Pts',(4.52349444223894,1.91148615363887,-5.17945806639703));
#6417=CARTESIAN_POINT('Ctrl Pts',(4.53934342743911,1.91616677929283,-5.18050859076488));
#6418=CARTESIAN_POINT('Ctrl Pts',(4.54986475541454,1.91918009847527,-5.18119960800947));
#6419=CARTESIAN_POINT('Ctrl Pts',(4.64731731655288,1.94622480219857,-5.1875458738251));
#6420=CARTESIAN_POINT('Ctrl Pts',(4.73577126136325,1.96442411363878,-5.19291108914789));
#6421=CARTESIAN_POINT('Ctrl Pts',(4.97084173553032,1.99637583227205,-5.20683902370581));
#6422=CARTESIAN_POINT('Ctrl Pts',(5.11825368088441,2.00001087643513,-5.21527525205736));
#6423=CARTESIAN_POINT('Ctrl Pts',(5.3070452282168,1.98377665772296,-5.22676186821689));
#6424=CARTESIAN_POINT('Ctrl Pts',(5.34923553970442,1.97878698884587,-5.22937010927931));
#6425=CARTESIAN_POINT('Ctrl Pts',(5.40512783787735,1.97035959218224,-5.23289576224414));
#6426=CARTESIAN_POINT('Ctrl Pts',(5.41900053741939,1.96811770315274,-5.23377662301283));
#6427=CARTESIAN_POINT('Ctrl Pts',(5.44160151179112,1.9642198096068,-5.23522165382061));
#6428=CARTESIAN_POINT('Ctrl Pts',(5.45034460428841,1.96265171847022,-5.23578309968515));
#6429=CARTESIAN_POINT('Ctrl Pts',(5.46721373009004,1.95950976892486,-5.23687122144608));
#6430=CARTESIAN_POINT('Ctrl Pts',(5.47534102704791,1.95794362306406,-5.23739764737598));
#6431=CARTESIAN_POINT('Ctrl Pts',(5.49424672746183,1.95417827668302,-5.23862742713321));
#6432=CARTESIAN_POINT('Ctrl Pts',(5.50501707229167,1.95194042305006,-5.23933197378369));
#6433=CARTESIAN_POINT('Ctrl Pts',(5.53967787618224,1.94443903150109,-5.24161241682866));
#6434=CARTESIAN_POINT('Ctrl Pts',(5.56348944002623,1.93882522784069,-5.24319920677025));
#6435=CARTESIAN_POINT('Ctrl Pts',(5.76469480781892,1.88746517394931,-5.25678539002971));
#6436=CARTESIAN_POINT('Ctrl Pts',(5.93508144129706,1.81792512317405,-5.26959192125343));
#6437=CARTESIAN_POINT('Ctrl Pts',(6.14096963814191,1.69868297205753,-5.28613388575147));
#6438=CARTESIAN_POINT('Ctrl Pts',(6.18724241698336,1.66927349769524,-5.28992086259104));
#6439=CARTESIAN_POINT('Ctrl Pts',(6.2322442180908,1.63799699450132,-5.29363746883395));
#6440=CARTESIAN_POINT('',(3.93347817078403,1.62253437445172,-5.29363746883395));
#6441=CARTESIAN_POINT('Origin',(5.09382715545311,0.,-5.29363746883395));
#6442=CARTESIAN_POINT('Ctrl Pts',(3.93347817078403,1.62253437445172,-5.29363746883395));
#6443=CARTESIAN_POINT('Ctrl Pts',(3.8753734702366,1.5809810296682,-5.28907786112167));
#6444=CARTESIAN_POINT('Ctrl Pts',(3.81946032609053,1.53627216112948,-5.28451825340938));
#6445=CARTESIAN_POINT('Ctrl Pts',(3.76608398691568,1.48866572503776,-5.2799586456971));
#6446=CARTESIAN_POINT('Ctrl Pts',(3.71089420556803,1.43944187718194,-5.27524412693162));
#6447=CARTESIAN_POINT('Ctrl Pts',(3.65841713885386,1.38712029687635,-5.27052960816615));
#6448=CARTESIAN_POINT('Ctrl Pts',(3.60899742177806,1.33203161542603,-5.26581508940068));
#6449=CARTESIAN_POINT('Ctrl Pts',(3.56123575882214,1.27879118444419,-5.26125874489691));
#6450=CARTESIAN_POINT('Ctrl Pts',(3.51632984488522,1.22296676941307,-5.25670240039315));
#6451=CARTESIAN_POINT('Ctrl Pts',(3.47455215491635,1.16489314322674,-5.25214605588938));
#6452=CARTESIAN_POINT('Ctrl Pts',(3.4327735996344,1.10681831420061,-5.24758961701313));
#6453=CARTESIAN_POINT('Ctrl Pts',(3.39412366375182,1.04649455185753,-5.24303317813688));
#6454=CARTESIAN_POINT('Ctrl Pts',(3.35883245938466,0.984287034921393,-5.23847673926063));
#6455=CARTESIAN_POINT('Ctrl Pts',(3.32353109970894,0.922061617306017,-5.23391898923494));
#6456=CARTESIAN_POINT('Ctrl Pts',(3.29159061787254,0.857951764582268,-5.22936123920926));
#6457=CARTESIAN_POINT('Ctrl Pts',(3.26319532059391,0.792347554864684,-5.22480348918357));
#6458=CARTESIAN_POINT('Ctrl Pts',(3.23478426638423,0.726706940491822,-5.22024321000131));
#6459=CARTESIAN_POINT('Ctrl Pts',(3.20992248861641,0.659570739210518,-5.21568293081904));
#6460=CARTESIAN_POINT('Ctrl Pts',(3.18874577409805,0.591348030278524,-5.21112265163678));
#6461=CARTESIAN_POINT('Ctrl Pts',(3.16753641797883,0.523020163465085,-5.20655534328043));
#6462=CARTESIAN_POINT('Ctrl Pts',(3.15002359695028,0.453602882957732,-5.20198803492408));
#6463=CARTESIAN_POINT('Ctrl Pts',(3.13629280128157,0.38351898875835,-5.19742072656773));
#6464=CARTESIAN_POINT('Ctrl Pts',(3.12254972380403,0.313372406495415,-5.19284933288308));
#6465=CARTESIAN_POINT('Ctrl Pts',(3.11259547387306,0.242558474210875,-5.18827793919843));
#6466=CARTESIAN_POINT('Ctrl Pts',(3.10646377784675,0.171506174375812,-5.18370654551377));
#6467=CARTESIAN_POINT('Ctrl Pts',(3.1003208348948,0.100323548456682,-5.179126766853));
#6468=CARTESIAN_POINT('Ctrl Pts',(3.09801445824188,0.0289021375374889,-5.17454698819222));
#6469=CARTESIAN_POINT('Ctrl Pts',(3.09952631099107,-0.0423285279449318,
-5.16996720953145));
#6470=CARTESIAN_POINT('Ctrl Pts',(3.09987370336958,-0.0586958562568392,
-5.16891487146288));
#6471=CARTESIAN_POINT('Ctrl Pts',(3.10042247643775,-0.0750531374033765,
-5.16786253339431));
#6472=CARTESIAN_POINT('Ctrl Pts',(3.10117202283689,-0.0913952129941374,
-5.16681019532573));
#6473=CARTESIAN_POINT('Ctrl Pts',(3.10431305765046,-0.159878002605746,-5.16240028752975));
#6474=CARTESIAN_POINT('Ctrl Pts',(3.11099626812022,-0.228362232762861,-5.15799037973377));
#6475=CARTESIAN_POINT('Ctrl Pts',(3.12122800980039,-0.296445902434433,-5.15358047193779));
#6476=CARTESIAN_POINT('Ctrl Pts',(3.13144268768317,-0.364416026828859,-5.14917791868373));
#6477=CARTESIAN_POINT('Ctrl Pts',(3.1451940865303,-0.43198642593221,-5.14477536542967));
#6478=CARTESIAN_POINT('Ctrl Pts',(3.16243659052121,-0.498756501904512,-5.14037281217561));
#6479=CARTESIAN_POINT('Ctrl Pts',(3.17965548824249,-0.56543516467969,-5.13597628634421));
#6480=CARTESIAN_POINT('Ctrl Pts',(3.20035587887727,-0.631315197845588,-5.1315797605128));
#6481=CARTESIAN_POINT('Ctrl Pts',(3.22444081749529,-0.696004512885265,-5.12718323468139));
#6482=CARTESIAN_POINT('Ctrl Pts',(3.24850784884,-0.760645731093032,-5.12278997768911));
#6483=CARTESIAN_POINT('Ctrl Pts',(3.27595426613844,-0.824097518387005,-5.11839672069683));
#6484=CARTESIAN_POINT('Ctrl Pts',(3.3066332883872,-0.885982868921297,-5.11400346370455));
#6485=CARTESIAN_POINT('Ctrl Pts',(3.33730044834284,-0.947844290982176,-5.10961190540077));
#6486=CARTESIAN_POINT('Ctrl Pts',(3.37119751199032,-1.00814002943846,-5.10522034709698));
#6487=CARTESIAN_POINT('Ctrl Pts',(3.40813033188671,-1.06651478260648,-5.1008287887932));
#6488=CARTESIAN_POINT('Ctrl Pts',(3.44506205012717,-1.12488779453478,-5.09643736148364));
#6489=CARTESIAN_POINT('Ctrl Pts',(3.48502907526759,-1.18133951304622,-5.09204593417409));
#6490=CARTESIAN_POINT('Ctrl Pts',(3.52779326149865,-1.23554255510922,-5.08765450686453));
#6491=CARTESIAN_POINT('Ctrl Pts',(3.57060072355836,-1.28980044871432,-5.08325863558743));
#6492=CARTESIAN_POINT('Ctrl Pts',(3.61621068605795,-1.34180472978312,-5.07886276431032));
#6493=CARTESIAN_POINT('Ctrl Pts',(3.66434462067253,-1.39126102700295,-5.07446689303322));
#6494=CARTESIAN_POINT('Ctrl Pts',(3.7125047053187,-1.44074419266277,-5.07006863358292));
#6495=CARTESIAN_POINT('Ctrl Pts',(3.7631911220563,-1.48767628083195,-5.06567037413261));
#6496=CARTESIAN_POINT('Ctrl Pts',(3.81609053451927,-1.53180177895985,-5.06127211468231));
#6497=CARTESIAN_POINT('Ctrl Pts',(3.86908438967676,-1.57600605548522,-5.05686600290521));
#6498=CARTESIAN_POINT('Ctrl Pts',(3.92429872536512,-1.61739344136932,-5.05245989112812));
#6499=CARTESIAN_POINT('Ctrl Pts',(3.98139012068197,-1.6557510097142,-5.04805377935102));
#6500=CARTESIAN_POINT('Ctrl Pts',(4.01624901224758,-1.67917139221202,-5.04536349350652));
#6501=CARTESIAN_POINT('Ctrl Pts',(4.05180715926841,-1.70146311100992,-5.04267320766202));
#6502=CARTESIAN_POINT('Ctrl Pts',(4.08798226477829,-1.72258631667715,-5.03998292181752));
#6503=CARTESIAN_POINT('Ctrl Pts',(4.14798585362447,-1.75762334366313,-5.03552054904992));
#6504=CARTESIAN_POINT('Ctrl Pts',(4.20993801918174,-1.78958901750203,-5.03105817628233));
#6505=CARTESIAN_POINT('Ctrl Pts',(4.27349218707037,-1.8182623853967,-5.02659580351474));
#6506=CARTESIAN_POINT('Ctrl Pts',(4.33695161079536,-1.84689300811272,-5.02214008308466));
#6507=CARTESIAN_POINT('Ctrl Pts',(4.40200785542346,-1.87224086854705,-5.01768436265459));
#6508=CARTESIAN_POINT('Ctrl Pts',(4.46828841563392,-1.89413010310417,-5.01322864222452));
#6509=CARTESIAN_POINT('Ctrl Pts',(4.53449120533457,-1.9159936538571,-5.00877814992844));
#6510=CARTESIAN_POINT('Ctrl Pts',(4.60191499636852,-1.9344064878101,-5.00432765763235));
#6511=CARTESIAN_POINT('Ctrl Pts',(4.67016754203147,-1.94924090210918,-4.99987716533626));
#6512=CARTESIAN_POINT('Ctrl Pts',(4.73837720656159,-1.96406599636777,-4.99542946915788));
#6513=CARTESIAN_POINT('Ctrl Pts',(4.80741411742909,-1.97531702834745,-4.9909817729795));
#6514=CARTESIAN_POINT('Ctrl Pts',(4.87687255648581,-1.98291660553008,-4.98653407680112));
#6515=CARTESIAN_POINT('Ctrl Pts',(4.94631070428743,-1.9905139626087,-4.98208767995136));
#6516=CARTESIAN_POINT('Ctrl Pts',(5.01616965151141,-1.99446192986204,-4.9776412831016));
#6517=CARTESIAN_POINT('Ctrl Pts',(5.08603695885747,-1.99473478822048,-4.97319488625183));
#6518=CARTESIAN_POINT('Ctrl Pts',(5.15590733943729,-1.99500765858106,-4.96874829381965));
#6519=CARTESIAN_POINT('Ctrl Pts',(5.22578559346422,-1.99160509957665,-4.96430170138747));
#6520=CARTESIAN_POINT('Ctrl Pts',(5.29525943375409,-1.98455350135956,-4.95985510895529));
#6521=CARTESIAN_POINT('Ctrl Pts',(5.36480480623327,-1.97749464262172,-4.95540393818844));
#6522=CARTESIAN_POINT('Ctrl Pts',(5.43394444802563,-1.96677929490471,-4.95095276742159));
#6523=CARTESIAN_POINT('Ctrl Pts',(5.50227230557564,-1.952485626539,-4.94650159665474));
#6524=CARTESIAN_POINT('Ctrl Pts',(5.5706393841556,-1.93818375343198,-4.94204787086117));
#6525=CARTESIAN_POINT('Ctrl Pts',(5.63819327947979,-1.92029959530799,-4.93759414506759));
#6526=CARTESIAN_POINT('Ctrl Pts',(5.70454189775908,-1.89896157571188,-4.93314041927402));
#6527=CARTESIAN_POINT('Ctrl Pts',(5.77100263307362,-1.87758749876361,-4.92867916749807));
#6528=CARTESIAN_POINT('Ctrl Pts',(5.83625357025589,-1.85274808319428,-4.92421791572212));
#6529=CARTESIAN_POINT('Ctrl Pts',(5.89992218843671,-1.82462005916278,-4.91975666394617));
#6530=CARTESIAN_POINT('Ctrl Pts',(5.93132425264772,-1.81074700769718,-4.91755632540055));
#6531=CARTESIAN_POINT('Ctrl Pts',(5.96234177917846,-1.79607469034805,-4.91535598685492));
#6532=CARTESIAN_POINT('Ctrl Pts',(5.99293249024594,-1.78062830468548,-4.9131556483093));
#6533=CARTESIAN_POINT('Ctrl Pts',(6.05498318767251,-1.74929660399475,-4.90869244570412));
#6534=CARTESIAN_POINT('Ctrl Pts',(6.11551123781745,-1.7146584687059,-4.90422924309895));
#6535=CARTESIAN_POINT('Ctrl Pts',(6.17414294624894,-1.67688561167934,-4.89976604049377));
#6536=CARTESIAN_POINT('Ctrl Pts',(6.23268933239712,-1.63916772262991,-4.89530933284921));
#6537=CARTESIAN_POINT('Ctrl Pts',(6.28934444840992,-1.59832442910512,-4.89085262520466));
#6538=CARTESIAN_POINT('Ctrl Pts',(6.34375847328421,-1.55457365962665,-4.8863959175601));
#6539=CARTESIAN_POINT('Ctrl Pts',(6.39811147169727,-1.5108719575466,-4.88194420820591));
#6540=CARTESIAN_POINT('Ctrl Pts',(6.45022799340618,-1.46426956035437,-4.87749249885171));
#6541=CARTESIAN_POINT('Ctrl Pts',(6.49978800489005,-1.41502708537701,-4.87304078949752));
#6542=CARTESIAN_POINT('Ctrl Pts',(6.5493184697692,-1.36581396769599,-4.86859173415596));
#6543=CARTESIAN_POINT('Ctrl Pts',(6.59629510362083,-1.31396423782261,-4.8641426788144));
#6544=CARTESIAN_POINT('Ctrl Pts',(6.64043287929411,-1.25977708245636,-4.85969362347284));
#6545=CARTESIAN_POINT('Ctrl Pts',(6.68455915814744,-1.20560404152971,-4.85524572700229));
#6546=CARTESIAN_POINT('Ctrl Pts',(6.72584773954907,-1.14909516160501,-4.85079783053173));
#6547=CARTESIAN_POINT('Ctrl Pts',(6.76405340047442,-1.0905832627278,-4.84634993406117));
#6548=CARTESIAN_POINT('Ctrl Pts',(6.80226193495501,-1.03206696300607,-4.8419017030518));
#6549=CARTESIAN_POINT('Ctrl Pts',(6.83738682424129,-0.971547754435772,-4.83745347204244));
#6550=CARTESIAN_POINT('Ctrl Pts',(6.86922673464641,-0.909386549658754,-4.83300524103307));
#6551=CARTESIAN_POINT('Ctrl Pts',(6.90110085428473,-0.847158558037083,-4.82855223078375));
#6552=CARTESIAN_POINT('Ctrl Pts',(6.92968272841109,-0.783285483644192,-4.82409922053443));
#6553=CARTESIAN_POINT('Ctrl Pts',(6.95481791846453,-0.718151058264328,-4.81964621028511));
#6554=CARTESIAN_POINT('Ctrl Pts',(6.97996819188313,-0.652977546395753,-4.81519052783083));
#6555=CARTESIAN_POINT('Ctrl Pts',(7.00166751287834,-0.586541640042753,-4.81073484537655));
#6556=CARTESIAN_POINT('Ctrl Pts',(7.01981125049916,-0.519242552310239,-4.80627916292227));
#6557=CARTESIAN_POINT('Ctrl Pts',(7.03798629550514,-0.451827338644638,-4.80181579209805));
#6558=CARTESIAN_POINT('Ctrl Pts',(7.05259340871707,-0.38354644677953,-4.79735242127384));
#6559=CARTESIAN_POINT('Ctrl Pts',(7.06357916381499,-0.314808811907094,-4.79288905044963));
#6560=CARTESIAN_POINT('Ctrl Pts',(7.06896179044333,-0.281129832125018,-4.79070215856678));
#6561=CARTESIAN_POINT('Ctrl Pts',(7.07347584890439,-0.247341274937136,-4.78851526668393));
#6562=CARTESIAN_POINT('Ctrl Pts',(7.07711961959692,-0.213491367905988,-4.78632837480109));
#6563=CARTESIAN_POINT('Ctrl Pts',(7.08469843048945,-0.143085717889515,-4.78177977901363));
#6564=CARTESIAN_POINT('Ctrl Pts',(7.08852952589302,-0.0722653690654421,
-4.77723118322618));
#6565=CARTESIAN_POINT('Ctrl Pts',(7.08857671412439,-0.00132690645140175,
-4.77268258743872));
#6566=CARTESIAN_POINT('Origin',(5.09382715545311,0.,-6.77268258743872));
#6567=CARTESIAN_POINT('',(7.08797499842338,0.00179838134685419,-3.81459200118186));
#6568=CARTESIAN_POINT('',(7.08573545875024,-0.000892991754021077,-3.97270035107971));
#6569=CARTESIAN_POINT('',(7.08857715545311,8.3550772080578E-14,-6.77268258743872));
#6570=CARTESIAN_POINT('Ctrl Pts',(7.08857636722083,0.00177331668636056,
-3.81424619860756));
#6571=CARTESIAN_POINT('Ctrl Pts',(7.08868493718784,-0.120353688486413,-3.82134987712496));
#6572=CARTESIAN_POINT('Ctrl Pts',(7.0775782485065,-0.242220620626991,-3.82853578695394));
#6573=CARTESIAN_POINT('Ctrl Pts',(7.0528391367539,-0.376162548922293,-3.83696215330685));
#6574=CARTESIAN_POINT('Ctrl Pts',(7.0501324847327,-0.389994421885436,-3.83783843504427));
#6575=CARTESIAN_POINT('Ctrl Pts',(7.04537824197903,-0.412994111282967,-3.83930629344508));
#6576=CARTESIAN_POINT('Ctrl Pts',(7.04341203446348,-0.422178367559234,-3.83989531658134));
#6577=CARTESIAN_POINT('Ctrl Pts',(7.03942356063078,-0.440186479087877,-3.84105608047177));
#6578=CARTESIAN_POINT('Ctrl Pts',(7.03740594259745,-0.449011137968301,-3.84162766169996));
#6579=CARTESIAN_POINT('Ctrl Pts',(7.03348124127359,-0.465654764271371,-3.84271104446087));
#6580=CARTESIAN_POINT('Ctrl Pts',(7.0315867624428,-0.473476540652351,-3.84322243317116));
#6581=CARTESIAN_POINT('Ctrl Pts',(7.02719449821022,-0.491142988340545,-3.8443826542762));
#6582=CARTESIAN_POINT('Ctrl Pts',(7.02466876780043,-0.50098041756057,-3.8450323725717));
#6583=CARTESIAN_POINT('Ctrl Pts',(7.01796762726499,-0.526276941322821,-3.84671273033162));
#6584=CARTESIAN_POINT('Ctrl Pts',(7.01368106020594,-0.541705578630841,-3.84774691855927));
#6585=CARTESIAN_POINT('Ctrl Pts',(6.98127167752794,-0.653137131235577,-3.85528557673982));
#6586=CARTESIAN_POINT('Ctrl Pts',(6.94615230061261,-0.746941140064223,-3.8620174191873));
#6587=CARTESIAN_POINT('Ctrl Pts',(6.87049712102965,-0.910436155184257,-3.87441783100382));
#6588=CARTESIAN_POINT('Ctrl Pts',(6.83249001261459,-0.981071208680531,-3.88001811585327));
#6589=CARTESIAN_POINT('Ctrl Pts',(6.74611470559416,-1.12073304743609,-3.89145471180277));
#6590=CARTESIAN_POINT('Ctrl Pts',(6.69740925624548,-1.18937950939001,-3.89727782484544));
#6591=CARTESIAN_POINT('Ctrl Pts',(6.63013691080471,-1.27251805247618,-3.90442338933991));
#6592=CARTESIAN_POINT('Ctrl Pts',(6.61545624457557,-1.29003677492584,-3.90593450432855));
#6593=CARTESIAN_POINT('Ctrl Pts',(6.59679140359883,-1.31154780974618,-3.90779278355947));
#6594=CARTESIAN_POINT('Ctrl Pts',(6.59308780056581,-1.31577988595263,-3.90815851825653));
#6595=CARTESIAN_POINT('Ctrl Pts',(6.58587134929426,-1.32395603410954,-3.90886526900823));
#6596=CARTESIAN_POINT('Ctrl Pts',(6.58236064031558,-1.32790192508087,-3.90920643186956));
#6597=CARTESIAN_POINT('Ctrl Pts',(6.57582655771295,-1.33518748762305,-3.90983641143045));
#6598=CARTESIAN_POINT('Ctrl Pts',(6.57280756088526,-1.33853084252206,-3.91012552783963));
#6599=CARTESIAN_POINT('Ctrl Pts',(6.56590189791195,-1.34612655489895,-3.91078243988307));
#6600=CARTESIAN_POINT('Ctrl Pts',(6.5620081225761,-1.35037231864342,-3.91114969484924));
#6601=CARTESIAN_POINT('Ctrl Pts',(6.55179519415034,-1.36141207868538,-3.91210497481531));
#6602=CARTESIAN_POINT('Ctrl Pts',(6.54544685250411,-1.3681790499666,-3.9126908759351));
#6603=CARTESIAN_POINT('Ctrl Pts',(6.50112739431156,-1.41476533167554,-3.91672895200675));
#6604=CARTESIAN_POINT('Ctrl Pts',(6.46156648239265,-1.45304687488431,-3.92007047626247));
#6605=CARTESIAN_POINT('Ctrl Pts',(6.38265470622991,-1.52332373244278,-3.92636966106398));
#6606=CARTESIAN_POINT('Ctrl Pts',(6.34356969428608,-1.55554995555016,-3.92933438178092));
#6607=CARTESIAN_POINT('Ctrl Pts',(6.20622524192424,-1.6602709941878,-3.9393916918384));
#6608=CARTESIAN_POINT('Ctrl Pts',(6.10256740660566,-1.7252161735282,-3.94640263768227));
#6609=CARTESIAN_POINT('Ctrl Pts',(5.94116771046996,-1.80679172218707,-3.95722480054487));
#6610=CARTESIAN_POINT('Ctrl Pts',(5.88756805845946,-1.83097152842719,-3.96080133028954));
#6611=CARTESIAN_POINT('Ctrl Pts',(5.81914381043214,-1.85826943915055,-3.96538605804275));
#6612=CARTESIAN_POINT('Ctrl Pts',(5.80524382536161,-1.86363512022709,-3.96631829902992));
#6613=CARTESIAN_POINT('Ctrl Pts',(5.78272865540576,-1.87203784686826,-3.96783034836368));
#6614=CARTESIAN_POINT('Ctrl Pts',(5.77415027143917,-1.87517237344433,-3.96840691052599));
#6615=CARTESIAN_POINT('Ctrl Pts',(5.7579836003182,-1.8809541103729,-3.96949449668728));
#6616=CARTESIAN_POINT('Ctrl Pts',(5.75040022957682,-1.88361459535506,-3.97000506918895));
#6617=CARTESIAN_POINT('Ctrl Pts',(5.73331489358926,-1.88949295722637,-3.97115641524462));
#6618=CARTESIAN_POINT('Ctrl Pts',(5.72380436832726,-1.89268510530384,-3.97179802032093));
#6619=CARTESIAN_POINT('Ctrl Pts',(5.69944211943663,-1.9006581763267,-3.97344355688786));
#6620=CARTESIAN_POINT('Ctrl Pts',(5.68455786463766,-1.90533676661088,-3.97445079471311));
#6621=CARTESIAN_POINT('Ctrl Pts',(5.58632702583627,-1.93495216274059,-3.98111194071517));
#6622=CARTESIAN_POINT('Ctrl Pts',(5.50149138906808,-1.95458492288619,-3.98693566383776));
#6623=CARTESIAN_POINT('Ctrl Pts',(5.27090091917171,-1.99228165763517,-4.00292625774647));
#6624=CARTESIAN_POINT('Ctrl Pts',(5.123990446511,-1.99990687132354,-4.01331056366706));
#6625=CARTESIAN_POINT('Ctrl Pts',(4.92726552521078,-1.98842267231143,-4.02678734633476));
#6626=CARTESIAN_POINT('Ctrl Pts',(4.8770778572172,-1.98357964055613,-4.03018296403609));
#6627=CARTESIAN_POINT('Ctrl Pts',(4.81763726118323,-1.97556025633291,-4.03411413998269));
#6628=CARTESIAN_POINT('Ctrl Pts',(4.80816039167025,-1.97421217019396,-4.03473813676925));
#6629=CARTESIAN_POINT('Ctrl Pts',(4.79348107021089,-1.97201611750034,-4.03570000937651));
#6630=CARTESIAN_POINT('Ctrl Pts',(4.78827180894577,-1.97121568337227,-4.03604043474387));
#6631=CARTESIAN_POINT('Ctrl Pts',(4.77861426088005,-1.96969253993504,-4.03666978051929));
#6632=CARTESIAN_POINT('Ctrl Pts',(4.77416527832216,-1.96897540759155,-4.03695899494));
#6633=CARTESIAN_POINT('Ctrl Pts',(4.76401797969515,-1.96730446261442,-4.03761705428538));
#6634=CARTESIAN_POINT('Ctrl Pts',(4.75832135502093,-1.96634096761489,-4.03798535124291));
#6635=CARTESIAN_POINT('Ctrl Pts',(4.74343391393133,-1.96375640927986,-4.03894507509495));
#6636=CARTESIAN_POINT('Ctrl Pts',(4.73425002332634,-1.96209555135703,-4.0395343463408));
#6637=CARTESIAN_POINT('Ctrl Pts',(4.66973361276343,-1.94995989640804,-4.04365658295084));
#6638=CARTESIAN_POINT('Ctrl Pts',(4.61484932978633,-1.93720944384359,-4.0470736057074));
#6639=CARTESIAN_POINT('Ctrl Pts',(4.40425669863946,-1.87878568108783,-4.06008933401293));
#6640=CARTESIAN_POINT('Ctrl Pts',(4.25381105548481,-1.81651348921816,-4.06923032570495));
#6641=CARTESIAN_POINT('Ctrl Pts',(4.05395446586769,-1.70359140747278,-4.08289707375988));
#6642=CARTESIAN_POINT('Ctrl Pts',(3.99706650806883,-1.66753517257291,-4.08697697801182));
#6643=CARTESIAN_POINT('Ctrl Pts',(3.92938752943551,-1.61967615849919,-4.09213331696542));
#6644=CARTESIAN_POINT('Ctrl Pts',(3.91676766747666,-1.61052831120532,-4.09310832881417));
#6645=CARTESIAN_POINT('Ctrl Pts',(3.89693642513926,-1.59579550723166,-4.09466278238691));
#6646=CARTESIAN_POINT('Ctrl Pts',(3.88965375041438,-1.59030724306958,-4.09523848243564));
#6647=CARTESIAN_POINT('Ctrl Pts',(3.87602227143736,-1.57988716475571,-4.09632537556468));
#6648=CARTESIAN_POINT('Ctrl Pts',(3.86966513234895,-1.57496651614995,-4.09683612410842));
#6649=CARTESIAN_POINT('Ctrl Pts',(3.85542426677458,-1.5638052768759,-4.09798911518404));
#6650=CARTESIAN_POINT('Ctrl Pts',(3.84755767758726,-1.55754327102538,-4.09863219886563));
#6651=CARTESIAN_POINT('Ctrl Pts',(3.82754888121719,-1.54136712448305,-4.10028397909205));
#6652=CARTESIAN_POINT('Ctrl Pts',(3.81547576639889,-1.53136898987631,-4.10129602423558));
#6653=CARTESIAN_POINT('Ctrl Pts',(3.73532588951009,-1.4633859701508,-4.10812018908574));
#6654=CARTESIAN_POINT('Ctrl Pts',(3.67110615960361,-1.4010300534179,-4.11411216139587));
#6655=CARTESIAN_POINT('Ctrl Pts',(3.52400899548458,-1.23762591005276,-4.12917603371625));
#6656=CARTESIAN_POINT('Ctrl Pts',(3.44645445508747,-1.13234580086618,-4.13837704949277));
#6657=CARTESIAN_POINT('Ctrl Pts',(3.34745233602156,-0.96601574092247,-4.15170837516356));
#6658=CARTESIAN_POINT('Ctrl Pts',(3.31775838737324,-0.910270751724883,-4.15599226510809));
#6659=CARTESIAN_POINT('Ctrl Pts',(3.28643662159656,-0.844078775114153,-4.1607966931851));
#6660=CARTESIAN_POINT('Ctrl Pts',(3.28218694873499,-0.834918733842127,-4.16145545305156));
#6661=CARTESIAN_POINT('Ctrl Pts',(3.27577877584355,-0.820826793237541,-4.16245913091229));
#6662=CARTESIAN_POINT('Ctrl Pts',(3.27357045047088,-0.815917927681905,-4.16280695353903));
#6663=CARTESIAN_POINT('Ctrl Pts',(3.26955379137893,-0.806891861208777,-4.16344311837032));
#6664=CARTESIAN_POINT('Ctrl Pts',(3.26773951123744,-0.80277749034145,-4.16373180931219));
#6665=CARTESIAN_POINT('Ctrl Pts',(3.26368424215999,-0.793496185649858,-4.16438015754031));
#6666=CARTESIAN_POINT('Ctrl Pts',(3.26145121594805,-0.788325883062689,-4.16473933246207));
#6667=CARTESIAN_POINT('Ctrl Pts',(3.25494093675585,-0.773074994649688,-4.16579311955614));
#6668=CARTESIAN_POINT('Ctrl Pts',(3.25072467741744,-0.762968374747399,-4.16648418196291));
#6669=CARTESIAN_POINT('Ctrl Pts',(3.21018688627579,-0.663499552197041,-4.17321933987693));
#6670=CARTESIAN_POINT('Ctrl Pts',(3.18030430087733,-0.571635951841423,-4.17892031083755));
#6671=CARTESIAN_POINT('Ctrl Pts',(3.12644801056572,-0.353415784629972,-4.19203644737749));
#6672=CARTESIAN_POINT('Ctrl Pts',(3.10779738484874,-0.226203569255492,-4.19938133297649));
#6673=CARTESIAN_POINT('Ctrl Pts',(3.09850310754975,-0.0374104867927232,
-4.21068151259365));
#6674=CARTESIAN_POINT('Ctrl Pts',(3.09828944129431,0.0233613286147556,-4.21437541613127));
#6675=CARTESIAN_POINT('Ctrl Pts',(3.10148552692239,0.0991515865623322,-4.21909717287567));
#6676=CARTESIAN_POINT('Ctrl Pts',(3.10229435119605,0.114250915461581,-4.22004349623843));
#6677=CARTESIAN_POINT('Ctrl Pts',(3.10385933329893,0.138336244660656,-4.2215626038634));
#6678=CARTESIAN_POINT('Ctrl Pts',(3.10450490849791,0.14732903061136,-4.22213193519071));
#6679=CARTESIAN_POINT('Ctrl Pts',(3.10584248378942,0.164345241550075,-4.22321341087904));
#6680=CARTESIAN_POINT('Ctrl Pts',(3.10652215277935,0.172369476507214,-4.22372515968712));
#6681=CARTESIAN_POINT('Ctrl Pts',(3.10817402036281,0.190561032868495,-4.22488943462558));
#6682=CARTESIAN_POINT('Ctrl Pts',(3.10917575155063,0.200725381397563,-4.22554287201069));
#6683=CARTESIAN_POINT('Ctrl Pts',(3.11196856105278,0.226994824268064,-4.22723939005901));
#6684=CARTESIAN_POINT('Ctrl Pts',(3.11387787646451,0.243086333343761,-4.22828613567068));
#6685=CARTESIAN_POINT('Ctrl Pts',(3.13290023444264,0.388264453519185,-4.23780011921221));
#6686=CARTESIAN_POINT('Ctrl Pts',(3.16241581569613,0.515385773439488,-4.24666487721178));
#6687=CARTESIAN_POINT('Ctrl Pts',(3.23394076493474,0.727006276628773,-4.2621831004046));
#6688=CARTESIAN_POINT('Ctrl Pts',(3.26993821661244,0.813108287092982,-4.26872232569067));
#6689=CARTESIAN_POINT('Ctrl Pts',(3.33826630146429,0.948944690767107,-4.27917225756356));
#6690=CARTESIAN_POINT('Ctrl Pts',(3.36702388002236,1.00032084947295,-4.28315640945874));
#6691=CARTESIAN_POINT('Ctrl Pts',(3.40324799144324,1.05880520180743,-4.28766857034937));
#6692=CARTESIAN_POINT('Ctrl Pts',(3.40854518979459,1.06721650623256,-4.28831691433583));
#6693=CARTESIAN_POINT('Ctrl Pts',(3.41678921282733,1.08009254673717,-4.28930804957806));
#6694=CARTESIAN_POINT('Ctrl Pts',(3.4196914003144,1.08458547173938,-4.28965363760164));
#6695=CARTESIAN_POINT('Ctrl Pts',(3.42506764562894,1.09283553042148,-4.29028766654735));
#6696=CARTESIAN_POINT('Ctrl Pts',(3.42753633296724,1.09659595741381,-4.29057643997769));
#6697=CARTESIAN_POINT('Ctrl Pts',(3.4331465399791,1.10507901357269,-4.29122740153915));
#6698=CARTESIAN_POINT('Ctrl Pts',(3.43629549019093,1.1097966090267,-4.29158908898623));
#6699=CARTESIAN_POINT('Ctrl Pts',(3.44448421312517,1.12195193196274,-4.29252034520933));
#6700=CARTESIAN_POINT('Ctrl Pts',(3.44955425250108,1.12936925173042,-4.29308796102699));
#6701=CARTESIAN_POINT('Ctrl Pts',(3.4825895103442,1.17700481783655,-4.29673087141259));
#6702=CARTESIAN_POINT('Ctrl Pts',(3.5119805100421,1.21621920137834,-4.29971861923559));
#6703=CARTESIAN_POINT('Ctrl Pts',(3.64916115070864,1.38585166332398,-4.31278605982088));
#6704=CARTESIAN_POINT('Ctrl Pts',(3.77183710688056,1.5033278697646,-4.32228755490991));
#6705=CARTESIAN_POINT('Ctrl Pts',(3.96282247149054,1.64454420090413,-4.33642005677532));
#6706=CARTESIAN_POINT('Ctrl Pts',(4.01981463453745,1.68231770048992,-4.34055964339273));
#6707=CARTESIAN_POINT('Ctrl Pts',(4.09210227260022,1.72505647156196,-4.3457830575649));
#6708=CARTESIAN_POINT('Ctrl Pts',(4.10566921889857,1.73286365347448,-4.3467621500912));
#6709=CARTESIAN_POINT('Ctrl Pts',(4.12729559522146,1.74497212682861,-4.34832160300116));
#6710=CARTESIAN_POINT('Ctrl Pts',(4.13529528864739,1.7493792145158,-4.34889817917964));
#6711=CARTESIAN_POINT('Ctrl Pts',(4.15039056410396,1.75756068176564,-4.34998579424775));
#6712=CARTESIAN_POINT('Ctrl Pts',(4.15747926133873,1.76134743026092,-4.35049638164129));
#6713=CARTESIAN_POINT('Ctrl Pts',(4.1734678037457,1.76976463765027,-4.35164776450256));
#6714=CARTESIAN_POINT('Ctrl Pts',(4.18238003623957,1.77437097354945,-4.3522893915366));
#6715=CARTESIAN_POINT('Ctrl Pts',(4.20524093135888,1.78596907286016,-4.35393499202639));
#6716=CARTESIAN_POINT('Ctrl Pts',(4.21923736567524,1.79286465847605,-4.35494227196329));
#6717=CARTESIAN_POINT('Ctrl Pts',(4.31162263322291,1.8370406140559,-4.36159082484642));
#6718=CARTESIAN_POINT('Ctrl Pts',(4.39228216209262,1.86932959433386,-4.3674010995762));
#6719=CARTESIAN_POINT('Ctrl Pts',(4.60097563057918,1.9374591449058,-4.38242403563893));
#6720=CARTESIAN_POINT('Ctrl Pts',(4.73095965921986,1.965953754757,-4.3917883529302));
#6721=CARTESIAN_POINT('Ctrl Pts',(4.92590347328156,1.98868418719369,-4.40530812282914));
#6722=CARTESIAN_POINT('Ctrl Pts',(4.98932484977301,1.99302386922152,-4.4096206742469));
#6723=CARTESIAN_POINT('Ctrl Pts',(5.06296160025615,1.99453682379001,-4.4144530046761));
#6724=CARTESIAN_POINT('Ctrl Pts',(5.07307359673255,1.9946676725813,-4.41511275463619));
#6725=CARTESIAN_POINT('Ctrl Pts',(5.088572611292,1.9947503513828,-4.41611765195087));
#6726=CARTESIAN_POINT('Ctrl Pts',(5.09395899178952,1.99475726815225,-4.41646571376282));
#6727=CARTESIAN_POINT('Ctrl Pts',(5.10384442531742,1.99472992109081,-4.41710226978938));
#6728=CARTESIAN_POINT('Ctrl Pts',(5.10834332566282,1.99470225481539,-4.41739111313872));
#6729=CARTESIAN_POINT('Ctrl Pts',(5.11847566830532,1.99460566321285,-4.41803973591781));
#6730=CARTESIAN_POINT('Ctrl Pts',(5.12410892732,1.99452809382701,-4.41839903324672));
#6731=CARTESIAN_POINT('Ctrl Pts',(5.14068631937358,1.9942295758479,-4.41945268718569));
#6732=CARTESIAN_POINT('Ctrl Pts',(5.15162925705423,1.99394240443241,-4.42014350154778));
#6733=CARTESIAN_POINT('Ctrl Pts',(5.25327424289737,1.99043746697274,-4.42652099039321));
#6734=CARTESIAN_POINT('Ctrl Pts',(5.34367229657635,1.9811225154274,-4.43190471483805));
#6735=CARTESIAN_POINT('Ctrl Pts',(5.54777118497731,1.94589212340713,-4.44401492948166));
#6736=CARTESIAN_POINT('Ctrl Pts',(5.66045713842258,1.91611367525903,-4.4506785048057));
#6737=CARTESIAN_POINT('Ctrl Pts',(5.84171755960184,1.85081434792718,-4.46209033508492));
#6738=CARTESIAN_POINT('Ctrl Pts',(5.91197809981789,1.82084619297313,-4.4666960616515));
#6739=CARTESIAN_POINT('Ctrl Pts',(5.99479658747012,1.77975895382683,-4.4724429589768));
#6740=CARTESIAN_POINT('Ctrl Pts',(6.00916133940246,1.77241393554925,-4.47345165386652));
#6741=CARTESIAN_POINT('Ctrl Pts',(6.031610821903,1.76058931737076,-4.47504763724565));
#6742=CARTESIAN_POINT('Ctrl Pts',(6.03975641510934,1.75622628969103,-4.47563083371797));
#6743=CARTESIAN_POINT('Ctrl Pts',(6.05492279210039,1.74796659327411,-4.47672454149934));
#6744=CARTESIAN_POINT('Ctrl Pts',(6.06195095616856,1.74408381031365,-4.47723455267584));
#6745=CARTESIAN_POINT('Ctrl Pts',(6.07758496186762,1.73532302304659,-4.47837628555783));
#6746=CARTESIAN_POINT('Ctrl Pts',(6.08617829904213,1.73042324822964,-4.47900877606706));
#6747=CARTESIAN_POINT('Ctrl Pts',(6.10782798142887,1.71786466512814,-4.48061494645639));
#6748=CARTESIAN_POINT('Ctrl Pts',(6.12083406796983,1.7101208915003,-4.48159166463867));
#6749=CARTESIAN_POINT('Ctrl Pts',(6.19852213728233,1.66265983516997,-4.48749845659424));
#6750=CARTESIAN_POINT('Ctrl Pts',(6.26097462679387,1.61942985221343,-4.49255628981042));
#6751=CARTESIAN_POINT('Ctrl Pts',(6.43330008936526,1.48499045910724,-4.50742883549091));
#6752=CARTESIAN_POINT('Ctrl Pts',(6.53604904064144,1.38541491083227,-4.51750004466973));
#6753=CARTESIAN_POINT('Ctrl Pts',(6.66910944272399,1.22547536809944,-4.53184440186276));
#6754=CARTESIAN_POINT('Ctrl Pts',(6.70844069098723,1.17317054895337,-4.53628844546908));
#6755=CARTESIAN_POINT('Ctrl Pts',(6.75084211033075,1.1106000704371,-4.54124810129733));
#6756=CARTESIAN_POINT('Ctrl Pts',(6.75648530422564,1.10213382487608,-4.5419119406784));
#6757=CARTESIAN_POINT('Ctrl Pts',(6.76502372598777,1.08910914804173,-4.54292173403489));
#6758=CARTESIAN_POINT('Ctrl Pts',(6.76796553514449,1.08458167097817,-4.54327064582244));
#6759=CARTESIAN_POINT('Ctrl Pts',(6.77332205535212,1.07626420417809,-4.54390771528552));
#6760=CARTESIAN_POINT('Ctrl Pts',(6.77574234410805,1.07247799745834,-4.54419623095214));
#6761=CARTESIAN_POINT('Ctrl Pts',(6.78115401660499,1.06394880909253,-4.54484285365857));
#6762=CARTESIAN_POINT('Ctrl Pts',(6.78413820345533,1.05920138197598,-4.54520048849706));
#6763=CARTESIAN_POINT('Ctrl Pts',(6.79174440372774,1.046986961271,-4.5461149607564));
#6764=CARTESIAN_POINT('Ctrl Pts',(6.79633725607806,1.03950182442264,-4.54666995626584));
#6765=CARTESIAN_POINT('Ctrl Pts',(6.8242986707766,0.993249637249924,-4.55006783406308));
#6766=CARTESIAN_POINT('Ctrl Pts',(6.84639343582795,0.953723565624938,-4.55283600584275));
#6767=CARTESIAN_POINT('Ctrl Pts',(6.91835306494699,0.814030984313544,-4.56227756185806));
#6768=CARTESIAN_POINT('Ctrl Pts',(6.96112787857238,0.710445508161588,-4.56869742606057));
#6769=CARTESIAN_POINT('Ctrl Pts',(6.99966731673572,0.589100303223355,-4.57610185468638));
#6770=CARTESIAN_POINT('Ctrl Pts',(7.00416936418842,0.574333115412954,-4.57700085377444));
#6771=CARTESIAN_POINT('Ctrl Pts',(7.03938958154149,0.453808827565126,-4.58432928193687));
#6772=CARTESIAN_POINT('Ctrl Pts',(7.06146908121588,0.345740020740353,-4.59085955017007));
#6773=CARTESIAN_POINT('Ctrl Pts',(7.07643856747226,0.220322586196322,-4.59869211625329));
#6774=CARTESIAN_POINT('Ctrl Pts',(7.07816260134698,0.204212798742335,-4.59970262358146));
#6775=CARTESIAN_POINT('Ctrl Pts',(7.08065269348092,0.177921473039154,-4.60135978374042));
#6776=CARTESIAN_POINT('Ctrl Pts',(7.08153717675632,0.167751703794786,-4.60200273626659));
#6777=CARTESIAN_POINT('Ctrl Pts',(7.08297916169725,0.149554672700093,-4.60315685237495));
#6778=CARTESIAN_POINT('Ctrl Pts',(7.083566228947,0.141529927553974,-4.60366708052049));
#6779=CARTESIAN_POINT('Ctrl Pts',(7.08470744144815,0.124516470237078,-4.60475161859928));
#6780=CARTESIAN_POINT('Ctrl Pts',(7.08524929550807,0.11552714074415,-4.60532630077847));
#6781=CARTESIAN_POINT('Ctrl Pts',(7.08653653892849,0.0914592334197121,-4.60686950727209));
#6782=CARTESIAN_POINT('Ctrl Pts',(7.08717163842198,0.0763755841462476,-4.60784144410451));
#6783=CARTESIAN_POINT('Ctrl Pts',(7.08826331049372,0.040860677808651,-4.6101416498511));
#6784=CARTESIAN_POINT('Ctrl Pts',(7.08857715560486,0.0204294355058518,-4.61147408152769));
#6785=CARTESIAN_POINT('Ctrl Pts',(7.08857715545311,-1.48167178722712E-8,
-4.61281584510352));
#6786=CARTESIAN_POINT('Ctrl Pts',(7.09088663849909,-0.00131116008061021,
-4.77268148053433));
#6787=CARTESIAN_POINT('Ctrl Pts',(7.08670907753058,0.587748466385314,-4.73495468745384));
#6788=CARTESIAN_POINT('Ctrl Pts',(6.49966055308458,1.84456991813218,-4.65495213653729));
#6789=CARTESIAN_POINT('Ctrl Pts',(4.36544687253163,2.24101253756461,-4.53267382778465));
#6790=CARTESIAN_POINT('Ctrl Pts',(2.81680518329998,0.606947674192248,-4.40584655427643));
#6791=CARTESIAN_POINT('Ctrl Pts',(3.34667777853599,-1.58138652746787,-4.27901928076822));
#6792=CARTESIAN_POINT('Ctrl Pts',(5.47143637460349,-2.32605244650467,-4.15219200726));
#6793=CARTESIAN_POINT('Ctrl Pts',(6.90460273165936,-1.21611912267368,-4.05008002852675));
#6794=CARTESIAN_POINT('Ctrl Pts',(7.08680593434348,-0.276931585723664,-3.99024380762958));
#6795=CARTESIAN_POINT('Ctrl Pts',(7.08570592294226,-0.000894131601634556,
-3.97268334456847));
#6796=CARTESIAN_POINT('Origin',(5.09382715545311,0.,-6.77268258743872));
#6797=CARTESIAN_POINT('',(7.08881171545261,-0.000532106017552724,-3.01459230695388));
#6798=CARTESIAN_POINT('',(7.08857715545311,1.10874632379271E-10,-3.17330009074087));
#6799=CARTESIAN_POINT('',(7.08857715545311,8.3550772080578E-14,-6.77268258743872));
#6800=CARTESIAN_POINT('Ctrl Pts',(7.08797499842339,0.00179838134685419,
-3.81459200118186));
#6801=CARTESIAN_POINT('Ctrl Pts',(7.08951448073131,0.176350806397102,-3.80345567575527));
#6802=CARTESIAN_POINT('Ctrl Pts',(6.98867393212712,1.01178905137383,-3.7500435924926));
#6803=CARTESIAN_POINT('Ctrl Pts',(5.81786592990346,2.24253293940595,-3.65435575139387));
#6804=CARTESIAN_POINT('Ctrl Pts',(3.6051149786703,1.82672505437059,-3.52752847788566));
#6805=CARTESIAN_POINT('Ctrl Pts',(2.75131773613265,-0.256588620430347,-3.40070120437744));
#6806=CARTESIAN_POINT('Ctrl Pts',(4.03585363174242,-2.10567795733919,-3.27387393086923));
#6807=CARTESIAN_POINT('Ctrl Pts',(6.28614853368186,-2.03262335577032,-3.147046657361));
#6808=CARTESIAN_POINT('Ctrl Pts',(7.07793075003761,-0.718427647632865,-3.06061946381432));
#6809=CARTESIAN_POINT('Ctrl Pts',(7.09175582045521,-0.0297929789795935,
-3.01646802810371));
#6810=CARTESIAN_POINT('Ctrl Pts',(7.09165120934631,-0.000533538361054326,
-3.01459235022917));
#6811=CARTESIAN_POINT('Ctrl Pts',(7.08857700164759,-0.000783330765841211,
-3.97433649156488));
#6812=CARTESIAN_POINT('Ctrl Pts',(7.08858993222558,0.0321443539113238,-3.97232913016949));
#6813=CARTESIAN_POINT('Ctrl Pts',(7.08778754968188,0.0650660683111326,-3.97029974614309));
#6814=CARTESIAN_POINT('Ctrl Pts',(7.08567929427801,0.107948074877877,-3.96762078150855));
#6815=CARTESIAN_POINT('Ctrl Pts',(7.08511261760091,0.117940376035509,-3.96699401838726));
#6816=CARTESIAN_POINT('Ctrl Pts',(7.0839699121099,0.135721644367752,-3.96587402092352));
#6817=CARTESIAN_POINT('Ctrl Pts',(7.08342328576995,0.143512341162737,-3.96538170510721));
#6818=CARTESIAN_POINT('Ctrl Pts',(7.08223840163136,0.159088984934294,-3.96439408001313));
#6819=CARTESIAN_POINT('Ctrl Pts',(7.08160012798591,0.166874791084507,-3.96389877871134));
#6820=CARTESIAN_POINT('Ctrl Pts',(7.08013644389767,0.183527303688283,-3.96283579569347));
#6821=CARTESIAN_POINT('Ctrl Pts',(7.07929736189154,0.192392608178248,-3.96226769674993));
#6822=CARTESIAN_POINT('Ctrl Pts',(7.07692440530385,0.21579265154685,-3.96076224303042));
#6823=CARTESIAN_POINT('Ctrl Pts',(7.07529012163093,0.230316446873925,-3.95982176948879));
#6824=CARTESIAN_POINT('Ctrl Pts',(7.06753280767526,0.293043653296804,-3.95573280238148));
#6825=CARTESIAN_POINT('Ctrl Pts',(7.05980966597646,0.341028854858834,-3.95253480437207));
#6826=CARTESIAN_POINT('Ctrl Pts',(7.01669226902968,0.558070234406168,-3.93774025471924));
#6827=CARTESIAN_POINT('Ctrl Pts',(6.96118721536257,0.722358738604517,-3.92553481354265));
#6828=CARTESIAN_POINT('Ctrl Pts',(6.85589416538907,0.937336689641738,-3.90902048885455));
#6829=CARTESIAN_POINT('Ctrl Pts',(6.82355122215285,0.995759412735924,-3.90448253037066));
#6830=CARTESIAN_POINT('Ctrl Pts',(6.78294760842785,1.06113335282907,-3.89943235118866));
#6831=CARTESIAN_POINT('Ctrl Pts',(6.77749163267361,1.06976905726683,-3.89876584521586));
#6832=CARTESIAN_POINT('Ctrl Pts',(6.76904652537039,1.08291128827571,-3.8977529126801));
#6833=CARTESIAN_POINT('Ctrl Pts',(6.76610510200148,1.08744805245059,-3.89740349895455));
#6834=CARTESIAN_POINT('Ctrl Pts',(6.76068422698521,1.09573503916655,-3.89676580078874));
#6835=CARTESIAN_POINT('Ctrl Pts',(6.75821054574705,1.09948883755708,-3.89647715618809));
#6836=CARTESIAN_POINT('Ctrl Pts',(6.7526248719228,1.10790301921835,-3.89583062489912));
#6837=CARTESIAN_POINT('Ctrl Pts',(6.74950592453,1.1125586634533,-3.89547320775268));
#6838=CARTESIAN_POINT('Ctrl Pts',(6.74030906444032,1.12616246319816,-3.89442956453444));
#6839=CARTESIAN_POINT('Ctrl Pts',(6.73417782383085,1.13507456459261,-3.89374678562785));
#6840=CARTESIAN_POINT('Ctrl Pts',(6.68342809355681,1.20757204789041,-3.88819632975819));
#6841=CARTESIAN_POINT('Ctrl Pts',(6.63519727213266,1.26855921146998,-3.8835498753102));
#6842=CARTESIAN_POINT('Ctrl Pts',(6.50868069598603,1.4106321278625,-3.8723659197789));
#6843=CARTESIAN_POINT('Ctrl Pts',(6.42685633738313,1.48819609835596,-3.86592679131834));
#6844=CARTESIAN_POINT('Ctrl Pts',(6.29106677821567,1.59668325024419,-3.85571217889294));
#6845=CARTESIAN_POINT('Ctrl Pts',(6.24147473212306,1.63269234490218,-3.8520682700016));
#6846=CARTESIAN_POINT('Ctrl Pts',(6.16881606508225,1.68050238198347,-3.84678210194602));
#6847=CARTESIAN_POINT('Ctrl Pts',(6.14705408841845,1.6942261807163,-3.84520538515987));
#6848=CARTESIAN_POINT('Ctrl Pts',(6.11299083244211,1.71479762096456,-3.84274349201212));
#6849=CARTESIAN_POINT('Ctrl Pts',(6.10087182240738,1.72194265426581,-3.84186877344927));
#6850=CARTESIAN_POINT('Ctrl Pts',(6.08054652717708,1.73363792853391,-3.84040312009163));
#6851=CARTESIAN_POINT('Ctrl Pts',(6.07238177413091,1.73825960066172,-3.83981472652832));
#6852=CARTESIAN_POINT('Ctrl Pts',(6.05641994815166,1.74714672025037,-3.83866497242767));
#6853=CARTESIAN_POINT('Ctrl Pts',(6.04862636374287,1.75141800103964,-3.8381038351006));
#6854=CARTESIAN_POINT('Ctrl Pts',(6.03378182708759,1.75942503285489,-3.83703536869395));
#6855=CARTESIAN_POINT('Ctrl Pts',(6.02673647636054,1.76317084450366,-3.83652840841744));
#6856=CARTESIAN_POINT('Ctrl Pts',(6.01076301772389,1.77154093381101,-3.83537923785553));
#6857=CARTESIAN_POINT('Ctrl Pts',(6.00182209278322,1.77614015307733,-3.83473616391758));
#6858=CARTESIAN_POINT('Ctrl Pts',(5.97885424654842,1.78773608606241,-3.83308442439851));
#6859=CARTESIAN_POINT('Ctrl Pts',(5.96477913785966,1.79463530739242,-3.83207241051087));
#6860=CARTESIAN_POINT('Ctrl Pts',(5.8701125143009,1.83966226605252,-3.82526572676097));
#6861=CARTESIAN_POINT('Ctrl Pts',(5.78713515336401,1.87251069987953,-3.81929234428525));
#6862=CARTESIAN_POINT('Ctrl Pts',(5.57781533754034,1.93955021582627,-3.80423490474391));
#6863=CARTESIAN_POINT('Ctrl Pts',(5.44977648105083,1.9670781670994,-3.79501963952288));
#6864=CARTESIAN_POINT('Ctrl Pts',(5.25722455434304,1.9890493242337,-3.78167185230354));
#6865=CARTESIAN_POINT('Ctrl Pts',(5.19416661123743,1.99322593016015,-3.77738547630428));
#6866=CARTESIAN_POINT('Ctrl Pts',(5.1209133435733,1.99459166082764,-3.77257858850057));
#6867=CARTESIAN_POINT('Ctrl Pts',(5.11081442342066,1.99470323557337,-3.77191971614666));
#6868=CARTESIAN_POINT('Ctrl Pts',(5.09533164637251,1.99475669647646,-3.77091588711614));
#6869=CARTESIAN_POINT('Ctrl Pts',(5.08994832165143,1.99475349302295,-3.77056802498463));
#6870=CARTESIAN_POINT('Ctrl Pts',(5.0800678169924,1.9947076147131,-3.7699317845504));
#6871=CARTESIAN_POINT('Ctrl Pts',(5.07557077484762,1.99467152507711,-3.76964305752163));
#6872=CARTESIAN_POINT('Ctrl Pts',(5.06544153262143,1.99455597687536,-3.76899462320745));
#6873=CARTESIAN_POINT('Ctrl Pts',(5.05980953229785,1.99446787180285,-3.76863539837715));
#6874=CARTESIAN_POINT('Ctrl Pts',(5.04322853715343,1.99413822946573,-3.76758148609537));
#6875=CARTESIAN_POINT('Ctrl Pts',(5.03228086341701,1.99383037519932,-3.76689034846135));
#6876=CARTESIAN_POINT('Ctrl Pts',(4.9310190255478,1.99014798867427,-3.7605366252053));
#6877=CARTESIAN_POINT('Ctrl Pts',(4.8410171710236,1.98072888231259,-3.75517460587202));
#6878=CARTESIAN_POINT('Ctrl Pts',(4.6369834338069,1.94523512794317,-3.74306500086495));
#6879=CARTESIAN_POINT('Ctrl Pts',(4.52399194383545,1.91518499455189,-3.73638239312475));
#6880=CARTESIAN_POINT('Ctrl Pts',(4.3423563464161,1.84937033842983,-3.72494097189099));
#6881=CARTESIAN_POINT('Ctrl Pts',(4.27200314493709,1.81919826501401,-3.72032580552199));
#6882=CARTESIAN_POINT('Ctrl Pts',(4.18911924232615,1.77786152321856,-3.7145684968291));
#6883=CARTESIAN_POINT('Ctrl Pts',(4.17476576028368,1.77048415179864,-3.71355952484302));
#6884=CARTESIAN_POINT('Ctrl Pts',(4.15233845347735,1.75861079955517,-3.71196336486479));
#6885=CARTESIAN_POINT('Ctrl Pts',(4.14420345675096,1.75423138339808,-3.71138027530926));
#6886=CARTESIAN_POINT('Ctrl Pts',(4.12905933882607,1.74594244769987,-3.71028692940035));
#6887=CARTESIAN_POINT('Ctrl Pts',(4.12204279563869,1.74204682073354,-3.70977717420887));
#6888=CARTESIAN_POINT('Ctrl Pts',(4.10643778929325,1.73325921124141,-3.70863622758977));
#6889=CARTESIAN_POINT('Ctrl Pts',(4.09786183922552,1.72834554902696,-3.70800426927988));
#6890=CARTESIAN_POINT('Ctrl Pts',(4.0762618443915,1.71575550345355,-3.70639986211648));
#6891=CARTESIAN_POINT('Ctrl Pts',(4.06328807751761,1.70799452515282,-3.7054243830952));
#6892=CARTESIAN_POINT('Ctrl Pts',(3.98599928660353,1.66055877116631,-3.69954067266061));
#6893=CARTESIAN_POINT('Ctrl Pts',(3.92390049598485,1.61740755442843,-3.69450579958175));
#6894=CARTESIAN_POINT('Ctrl Pts',(3.75183242852889,1.48273822803268,-3.67963995908714));
#6895=CARTESIAN_POINT('Ctrl Pts',(3.64906119601404,1.38278985345386,-3.66954923257848));
#6896=CARTESIAN_POINT('Ctrl Pts',(3.51610418073227,1.2223346134719,-3.65518154404755));
#6897=CARTESIAN_POINT('Ctrl Pts',(3.47684344556298,1.16990479189016,-3.65073340549605));
#6898=CARTESIAN_POINT('Ctrl Pts',(3.43453785635198,1.10719921993365,-3.64576988721702));
#6899=CARTESIAN_POINT('Ctrl Pts',(3.4289116705794,1.09872086056335,-3.64510599940647));
#6900=CARTESIAN_POINT('Ctrl Pts',(3.42039982936918,1.08567844869955,-3.64409618095095));
#6901=CARTESIAN_POINT('Ctrl Pts',(3.41746751816599,1.08114526211422,-3.6437472913967));
#6902=CARTESIAN_POINT('Ctrl Pts',(3.4121269961297,1.07281515246834,-3.64311009027123));
#6903=CARTESIAN_POINT('Ctrl Pts',(3.40971321918714,1.0690219959047,-3.6428214223522));
#6904=CARTESIAN_POINT('Ctrl Pts',(3.40431464611503,1.06047468253158,-3.64217426401934));
#6905=CARTESIAN_POINT('Ctrl Pts',(3.40133708472929,1.0557160763432,-3.64181624745534));
#6906=CARTESIAN_POINT('Ctrl Pts',(3.39265676719619,1.04171246573089,-3.64076915795914));
#6907=CARTESIAN_POINT('Ctrl Pts',(3.38700928376603,1.03243320194305,-3.64008356684079));
#6908=CARTESIAN_POINT('Ctrl Pts',(3.34002025264241,0.95378703963689,-3.63433798850469));
#6909=CARTESIAN_POINT('Ctrl Pts',(3.30284502838723,0.882006015624495,-3.62951731511248));
#6910=CARTESIAN_POINT('Ctrl Pts',(3.23241131827574,0.72306432332293,-3.61931185922023));
#6911=CARTESIAN_POINT('Ctrl Pts',(3.20070344996527,0.635432275023037,-3.61396285837639));
#6912=CARTESIAN_POINT('Ctrl Pts',(3.14844689698162,0.451775373412142,-3.6028055912222));
#6913=CARTESIAN_POINT('Ctrl Pts',(3.12863016439159,0.355812882930063,-3.5970011822122));
#6914=CARTESIAN_POINT('Ctrl Pts',(3.11288180620557,0.235450959331615,-3.5895202925018));
#6915=CARTESIAN_POINT('Ctrl Pts',(3.11024146469447,0.212059816794458,-3.58805770654022));
#6916=CARTESIAN_POINT('Ctrl Pts',(3.1070019000896,0.177954813195792,-3.58591016361791));
#6917=CARTESIAN_POINT('Ctrl Pts',(3.10607414336318,0.167273628059104,-3.58523544886738));
#6918=CARTESIAN_POINT('Ctrl Pts',(3.10459519640669,0.148491408908575,-3.5840450347101));
#6919=CARTESIAN_POINT('Ctrl Pts',(3.1040072740782,0.140393454010487,-3.58353049339193));
#6920=CARTESIAN_POINT('Ctrl Pts',(3.10295869636622,0.124617430199431,-3.58252547907882));
#6921=CARTESIAN_POINT('Ctrl Pts',(3.10249298002836,0.116939832233686,-3.58203517351227));
#6922=CARTESIAN_POINT('Ctrl Pts',(3.10136167173533,0.0963166106193942,-3.5807148126886));
#6923=CARTESIAN_POINT('Ctrl Pts',(3.1007778546204,0.0833670476668602,-3.57988222601684));
#6924=CARTESIAN_POINT('Ctrl Pts',(3.09907616894667,0.0351895253706318,-3.57677108310428));
#6925=CARTESIAN_POINT('Ctrl Pts',(3.09876586897419,-5.87062418391966E-5,
-3.57446771398511));
#6926=CARTESIAN_POINT('Ctrl Pts',(3.10295193581801,-0.236604242933865,-3.55881876194408));
#6927=CARTESIAN_POINT('Ctrl Pts',(3.13697600794851,-0.43619781027102,-3.54451610489363));
#6928=CARTESIAN_POINT('Ctrl Pts',(3.2177511839886,-0.680043507221302,-3.52689355388902));
#6929=CARTESIAN_POINT('Ctrl Pts',(3.23744019343108,-0.732085305721768,-3.52313511793488));
#6930=CARTESIAN_POINT('Ctrl Pts',(3.26313234579382,-0.792262777690295,-3.51884452549687));
#6931=CARTESIAN_POINT('Ctrl Pts',(3.26705077693763,-0.801256430455693,-3.51820479417909));
#6932=CARTESIAN_POINT('Ctrl Pts',(3.27319687370313,-0.815083588195336,-3.51722398695612));
#6933=CARTESIAN_POINT('Ctrl Pts',(3.27537773495614,-0.819937549609063,-3.51688020308298));
#6934=CARTESIAN_POINT('Ctrl Pts',(3.27943911162035,-0.82888108224929,-3.51624782126948));
#6935=CARTESIAN_POINT('Ctrl Pts',(3.28131403656732,-0.832972998766319,-3.5159589042967));
#6936=CARTESIAN_POINT('Ctrl Pts',(3.28559812583545,-0.842239823727202,-3.51530551953203));
#6937=CARTESIAN_POINT('Ctrl Pts',(3.28801565938601,-0.847410754495733,-3.51494156855519));
#6938=CARTESIAN_POINT('Ctrl Pts',(3.29434598363828,-0.860800752295372,-3.5140006106066));
#6939=CARTESIAN_POINT('Ctrl Pts',(3.29829294727148,-0.869003646418099,-3.51342562449494));
#6940=CARTESIAN_POINT('Ctrl Pts',(3.32490777979735,-0.923361170637173,-3.50962324021939));
#6941=CARTESIAN_POINT('Ctrl Pts',(3.34929895941641,-0.968655753052552,-3.50649239296052));
#6942=CARTESIAN_POINT('Ctrl Pts',(3.40397974408077,-1.06141756119578,-3.500055317874));
#6943=CARTESIAN_POINT('Ctrl Pts',(3.43458199702876,-1.10864675254,-3.49676288490253));
#6944=CARTESIAN_POINT('Ctrl Pts',(3.52662621919236,-1.23833433182978,-3.4875057813317));
#6945=CARTESIAN_POINT('Ctrl Pts',(3.59249788133462,-1.31742185275793,-3.4815900870162));
#6946=CARTESIAN_POINT('Ctrl Pts',(3.71638749223596,-1.44474717709875,-3.47105964525621));
#6947=CARTESIAN_POINT('Ctrl Pts',(3.77158094330595,-1.49542552453557,-3.4665383579411));
#6948=CARTESIAN_POINT('Ctrl Pts',(3.8419008013251,-1.55305039122955,-3.46088637790085));
#6949=CARTESIAN_POINT('Ctrl Pts',(3.85443576402625,-1.56307199743044,-3.45988293176198));
#6950=CARTESIAN_POINT('Ctrl Pts',(3.87435995341661,-1.5786108782361,-3.45829355531653));
#6951=CARTESIAN_POINT('Ctrl Pts',(3.88166902426058,-1.58423016702624,-3.45771166445687));
#6952=CARTESIAN_POINT('Ctrl Pts',(3.89541439575823,-1.59464693829044,-3.45661938833823));
#6953=CARTESIAN_POINT('Ctrl Pts',(3.90184123274415,-1.59945664442279,-3.45610949514641));
#6954=CARTESIAN_POINT('Ctrl Pts',(3.91626688393793,-1.61011725711222,-3.45496670753169));
#6955=CARTESIAN_POINT('Ctrl Pts',(3.92428057879507,-1.6159475777058,-3.45433303477855));
#6956=CARTESIAN_POINT('Ctrl Pts',(3.94469748097262,-1.63057035891761,-3.45272135238427));
#6957=CARTESIAN_POINT('Ctrl Pts',(3.95715820293689,-1.63928105442005,-3.45174026462255));
#6958=CARTESIAN_POINT('Ctrl Pts',(4.0337835790358,-1.69155247116689,-3.44572142003717));
#6959=CARTESIAN_POINT('Ctrl Pts',(4.10033637937241,-1.73147786638581,-3.44054998856304));
#6960=CARTESIAN_POINT('Ctrl Pts',(4.28024725452151,-1.82561471497388,-3.42672055652551));
#6961=CARTESIAN_POINT('Ctrl Pts',(4.39669640324256,-1.87317527946742,-3.41789999336075));
#6962=CARTESIAN_POINT('Ctrl Pts',(4.58677199626836,-1.93061169153583,-3.40413318805183));
#6963=CARTESIAN_POINT('Ctrl Pts',(4.65783200214184,-1.94789035456335,-3.39912375310112));
#6964=CARTESIAN_POINT('Ctrl Pts',(4.74459457097091,-1.96399951096233,-3.39328596934377));
#6965=CARTESIAN_POINT('Ctrl Pts',(4.75953434046229,-1.96659752470657,-3.39229065478195));
#6966=CARTESIAN_POINT('Ctrl Pts',(4.78076214081627,-1.97004011856314,-3.39089180103772));
#6967=CARTESIAN_POINT('Ctrl Pts',(4.78702637909183,-1.97102538248803,-3.39048089814288));
#6968=CARTESIAN_POINT('Ctrl Pts',(4.79782285215946,-1.97267077579039,-3.38977608496365));
#6969=CARTESIAN_POINT('Ctrl Pts',(4.80235282673824,-1.97334519399073,-3.38948138540015));
#6970=CARTESIAN_POINT('Ctrl Pts',(4.81118727152128,-1.9746293721628,-3.38890869566478));
#6971=CARTESIAN_POINT('Ctrl Pts',(4.81549142723941,-1.97524066500056,-3.3886306152164));
#6972=CARTESIAN_POINT('Ctrl Pts',(4.82728644585311,-1.97687651972526,-3.38787104436784));
#6973=CARTESIAN_POINT('Ctrl Pts',(4.83478128256406,-1.97787258543727,-3.38739112648365));
#6974=CARTESIAN_POINT('Ctrl Pts',(4.8639432205056,-1.98157960745624,-3.38553377648084));
#6975=CARTESIAN_POINT('Ctrl Pts',(4.88564949996013,-1.98397744943346,-3.38417267571356));
#6976=CARTESIAN_POINT('Ctrl Pts',(5.10213901983201,-2.00430017052009,-3.37077131297073));
#6977=CARTESIAN_POINT('Ctrl Pts',(5.29853933438375,-1.99384145272988,-3.35991850942686));
#6978=CARTESIAN_POINT('Ctrl Pts',(5.56187027551054,-1.94043723539433,-3.34397517767664));
#6979=CARTESIAN_POINT('Ctrl Pts',(5.63258554169497,-1.92200381385197,-3.33956146615471));
#6980=CARTESIAN_POINT('Ctrl Pts',(5.71730838863226,-1.89487541859839,-3.33403022736528));
#6981=CARTESIAN_POINT('Ctrl Pts',(5.73243157381938,-1.8898322872339,-3.33303334955274));
#6982=CARTESIAN_POINT('Ctrl Pts',(5.75618079220295,-1.88159501294759,-3.33145204822371));
#6983=CARTESIAN_POINT('Ctrl Pts',(5.76484816868126,-1.87852147395482,-3.3308715946752));
#6984=CARTESIAN_POINT('Ctrl Pts',(5.78104285137447,-1.87265229603755,-3.32978060695943));
#6985=CARTESIAN_POINT('Ctrl Pts',(5.78857515614601,-1.86987091721108,-3.3292705540238));
#6986=CARTESIAN_POINT('Ctrl Pts',(5.80539565481545,-1.86354411588399,-3.32812556449234));
#6987=CARTESIAN_POINT('Ctrl Pts',(5.81467449740856,-1.85997459790029,-3.3274898357398));
#6988=CARTESIAN_POINT('Ctrl Pts',(5.838170608212,-1.85073355144428,-3.32586938631766));
#6989=CARTESIAN_POINT('Ctrl Pts',(5.85234978798798,-1.84496754671929,-3.32488152905417));
#6990=CARTESIAN_POINT('Ctrl Pts',(5.94016131241538,-1.80807537455423,-3.31870021287182));
#6991=CARTESIAN_POINT('Ctrl Pts',(6.01192438444461,-1.77271336706427,-3.31336436481765));
#6992=CARTESIAN_POINT('Ctrl Pts',(6.20215390356457,-1.66432149526925,-3.29843363152046));
#6993=CARTESIAN_POINT('Ctrl Pts',(6.31541326412989,-1.58305925286827,-3.28862212492309));
#6994=CARTESIAN_POINT('Ctrl Pts',(6.46761856069933,-1.44772468949067,-3.27458440940185));
#6995=CARTESIAN_POINT('Ctrl Pts',(6.51383330665341,-1.40242430308452,-3.2701914895724));
#6996=CARTESIAN_POINT('Ctrl Pts',(6.56466366995959,-1.3475052952286,-3.26528138061859));
#6997=CARTESIAN_POINT('Ctrl Pts',(6.57150098647643,-1.34000396737603,-3.26461917911686));
#6998=CARTESIAN_POINT('Ctrl Pts',(6.58188365994687,-1.32843686026594,-3.26361137940618));
#6999=CARTESIAN_POINT('Ctrl Pts',(6.58547015733078,-1.32440847508855,-3.26326284020086));
#7000=CARTESIAN_POINT('Ctrl Pts',(6.59201658581576,-1.31699514461143,-3.26262597076471));
#7001=CARTESIAN_POINT('Ctrl Pts',(6.59498140824904,-1.3136147419634,-3.26233728676683));
#7002=CARTESIAN_POINT('Ctrl Pts',(6.60162607270662,-1.30598681780852,-3.26168970998422));
#7003=CARTESIAN_POINT('Ctrl Pts',(6.60529940526895,-1.30173376043301,-3.26133129391622));
#7004=CARTESIAN_POINT('Ctrl Pts',(6.61603915299017,-1.2891923152664,-3.26028195439781));
#7005=CARTESIAN_POINT('Ctrl Pts',(6.62305584883763,-1.28086135356562,-3.25959453508755));
#7006=CARTESIAN_POINT('Ctrl Pts',(6.69339043930943,-1.19595081401608,-3.25268013641715));
#7007=CARTESIAN_POINT('Ctrl Pts',(6.75097959073715,-1.1147880100955,-3.24681781204656));
#7008=CARTESIAN_POINT('Ctrl Pts',(6.86735574098765,-0.921691598572518,-3.23367211857729));
#7009=CARTESIAN_POINT('Ctrl Pts',(6.92204263515108,-0.807803146408631,-3.2264463077888));
#7010=CARTESIAN_POINT('Ctrl Pts',(6.9864311224792,-0.633011784159669,-3.21530642648322));
#7011=CARTESIAN_POINT('Ctrl Pts',(7.00467515583797,-0.575597567339887,-3.21164363434802));
#7012=CARTESIAN_POINT('Ctrl Pts',(7.02420599853337,-0.502884233737741,-3.20695688826785));
#7013=CARTESIAN_POINT('Ctrl Pts',(7.02795296092032,-0.48827490141617,-3.20601294937423));
#7014=CARTESIAN_POINT('Ctrl Pts',(7.03367268999514,-0.464874189902465,-3.20449672401071));
#7015=CARTESIAN_POINT('Ctrl Pts',(7.0357522305277,-0.456109316747675,-3.20392786594849));
#7016=CARTESIAN_POINT('Ctrl Pts',(7.03957883273296,-0.439480224269286,-3.20284668200946));
#7017=CARTESIAN_POINT('Ctrl Pts',(7.04133776628294,-0.431618899907222,-3.20233474734071));
#7018=CARTESIAN_POINT('Ctrl Pts',(7.04522223009477,-0.413750507549254,-3.20116921049005));
#7019=CARTESIAN_POINT('Ctrl Pts',(7.04731847817624,-0.403737371883485,-3.20051469029228));
#7020=CARTESIAN_POINT('Ctrl Pts',(7.05254626487011,-0.377771496048739,-3.19881365291587));
#7021=CARTESIAN_POINT('Ctrl Pts',(7.05555991950373,-0.361796060520636,-3.19776343951684));
#7022=CARTESIAN_POINT('Ctrl Pts',(7.07847589111606,-0.231601099446928,-3.18917300757686));
#7023=CARTESIAN_POINT('Ctrl Pts',(7.08857715545955,-0.11590233033206,-3.18132259334605));
#7024=CARTESIAN_POINT('Ctrl Pts',(7.08857715545311,1.10873879521911E-10,
-3.17330009074087));
#7025=CARTESIAN_POINT('Origin',(5.09382715545311,0.,-6.77268258743872));
#7026=CARTESIAN_POINT('',(7.08857665886015,-0.00140753592614233,-2.21459235027784));
#7027=CARTESIAN_POINT('',(7.08857712371927,-0.000258951665618427,-2.37086691085377));
#7028=CARTESIAN_POINT('',(7.08857715545311,8.3550772080578E-14,-6.77268258743872));
#7029=CARTESIAN_POINT('Ctrl Pts',(7.08857708451418,-0.000531987661214402,
-3.01459230337799));
#7030=CARTESIAN_POINT('Ctrl Pts',(7.08859546216608,0.0683771666358918,-3.01016806646156));
#7031=CARTESIAN_POINT('Ctrl Pts',(7.08503884163906,0.137429399923423,-3.00574382954513));
#7032=CARTESIAN_POINT('Ctrl Pts',(7.07788887578466,0.206219912750995,-3.00131959262871));
#7033=CARTESIAN_POINT('Ctrl Pts',(7.07062135308658,0.276141451338347,-2.9968226142002));
#7034=CARTESIAN_POINT('Ctrl Pts',(7.05964116392455,0.345792070396834,-2.9923256357717));
#7035=CARTESIAN_POINT('Ctrl Pts',(7.04498431714381,0.414744852750578,-2.98782865734319));
#7036=CARTESIAN_POINT('Ctrl Pts',(7.03060188308933,0.482406667048755,-2.98341587356644));
#7037=CARTESIAN_POINT('Ctrl Pts',(7.01267938170586,0.549396040749643,-2.97900308978969));
#7038=CARTESIAN_POINT('Ctrl Pts',(6.9913029820738,0.615315406836321,-2.97459030601294));
#7039=CARTESIAN_POINT('Ctrl Pts',(6.9699387309686,0.681197309963696,-2.97018003008705));
#7040=CARTESIAN_POINT('Ctrl Pts',(6.94512462731208,0.746009939868335,-2.96576975416116));
#7041=CARTESIAN_POINT('Ctrl Pts',(6.91699706735104,0.809369529232541,-2.96135947823527));
#7042=CARTESIAN_POINT('Ctrl Pts',(6.88887561533916,0.872715359950376,-2.95695016000856));
#7043=CARTESIAN_POINT('Ctrl Pts',(6.85744233713536,0.934608322762615,-2.95254084178185));
#7044=CARTESIAN_POINT('Ctrl Pts',(6.82288156633736,0.994685079159087,-2.94813152355514));
#7045=CARTESIAN_POINT('Ctrl Pts',(6.78712705327514,1.05683690973798,-2.9435699057876));
#7046=CARTESIAN_POINT('Ctrl Pts',(6.74802527877163,1.1170442563506,-2.93900828802005));
#7047=CARTESIAN_POINT('Ctrl Pts',(6.70583059911535,1.1749350876202,-2.9344466702525));
#7048=CARTESIAN_POINT('Ctrl Pts',(6.66499381394337,1.23096289632124,-2.93003185287914));
#7049=CARTESIAN_POINT('Ctrl Pts',(6.62126055726187,1.28482067694877,-2.92561703550578));
#7050=CARTESIAN_POINT('Ctrl Pts',(6.57490247950192,1.33620486714939,-2.92120221813241));
#7051=CARTESIAN_POINT('Ctrl Pts',(6.52623217107194,1.3901519785555,-2.91656720016777));
#7052=CARTESIAN_POINT('Ctrl Pts',(6.4746687918193,1.44137184772516,-2.91193218220313));
#7053=CARTESIAN_POINT('Ctrl Pts',(6.42056820986394,1.48955890687171,-2.90729716423849));
#7054=CARTESIAN_POINT('Ctrl Pts',(6.36646762790858,1.53774596601826,-2.90266214627385));
#7055=CARTESIAN_POINT('Ctrl Pts',(6.30983038151407,1.5828998882487,-2.89802712830921));
#7056=CARTESIAN_POINT('Ctrl Pts',(6.25104729766899,1.62476740026068,-2.89339211034457));
#7057=CARTESIAN_POINT('Ctrl Pts',(6.19454093398137,1.66501334698032,-2.88893661067226));
#7058=CARTESIAN_POINT('Ctrl Pts',(6.13582155018381,1.70238706390389,-2.88448111099996));
#7059=CARTESIAN_POINT('Ctrl Pts',(6.07521305597278,1.73663734750846,-2.88002561132766));
#7060=CARTESIAN_POINT('Ctrl Pts',(6.01469518919593,1.77083641691666,-2.87557677393114));
#7061=CARTESIAN_POINT('Ctrl Pts',(5.95229424110062,1.80192108422637,-2.87112793653462));
#7062=CARTESIAN_POINT('Ctrl Pts',(5.88836409443915,1.82968265420173,-2.86667909913811));
#7063=CARTESIAN_POINT('Ctrl Pts',(5.82450877432407,1.85741173086194,-2.86223546884896));
#7064=CARTESIAN_POINT('Ctrl Pts',(5.75912825713365,1.8818252414749,-2.85779183855981));
#7065=CARTESIAN_POINT('Ctrl Pts',(5.69260050297275,1.90276063675916,-2.85334820827066));
#7066=CARTESIAN_POINT('Ctrl Pts',(5.62611434793073,1.92368294135656,-2.84890735653773));
#7067=CARTESIAN_POINT('Ctrl Pts',(5.55848284459192,1.94113129864609,-2.8444665048048));
#7068=CARTESIAN_POINT('Ctrl Pts',(5.49010195824456,1.9549920314857,-2.84002565307186));
#7069=CARTESIAN_POINT('Ctrl Pts',(5.42174063850237,1.96884879819529,-2.83558607205063));
#7070=CARTESIAN_POINT('Ctrl Pts',(5.35263084063515,1.97911988133681,-2.8311464910294));
#7071=CARTESIAN_POINT('Ctrl Pts',(5.28317991413158,1.98574245441871,-2.82670691000816));
#7072=CARTESIAN_POINT('Ctrl Pts',(5.21372530700011,1.99236537847113,-2.82226709370647));
#7073=CARTESIAN_POINT('Ctrl Pts',(5.14393002252826,1.99533936456506,-2.81782727740478));
#7074=CARTESIAN_POINT('Ctrl Pts',(5.07420596529435,1.99465349657447,-2.81338746110309));
#7075=CARTESIAN_POINT('Ctrl Pts',(5.00440830903407,1.99396690459823,-2.80894295823883));
#7076=CARTESIAN_POINT('Ctrl Pts',(4.93468252017194,1.98961275280332,-2.80449845537456));
#7077=CARTESIAN_POINT('Ctrl Pts',(4.86543896293322,1.98163225549482,-2.8000539525103));
#7078=CARTESIAN_POINT('Ctrl Pts',(4.79615478586587,1.97364707664705,-2.79560684240066));
#7079=CARTESIAN_POINT('Ctrl Pts',(4.72735388594296,1.96203139957156,-2.79115973229101));
#7080=CARTESIAN_POINT('Ctrl Pts',(4.65943721402408,1.94687774174068,-2.78671262218137));
#7081=CARTESIAN_POINT('Ctrl Pts',(4.59140328371494,1.93169792106239,-2.78225783411935));
#7082=CARTESIAN_POINT('Ctrl Pts',(4.52425709972242,1.91296805832542,-2.77780304605733));
#7083=CARTESIAN_POINT('Ctrl Pts',(4.45838443394178,1.8908305344949,-2.7733482579953));
#7084=CARTESIAN_POINT('Ctrl Pts',(4.42494909585679,1.87959407419887,-2.77108711760899));
#7085=CARTESIAN_POINT('Ctrl Pts',(4.39184153906994,1.86748046069015,-2.76882597722268));
#7086=CARTESIAN_POINT('Ctrl Pts',(4.35910994638159,1.85451292397604,-2.76656483683636));
#7087=CARTESIAN_POINT('Ctrl Pts',(4.29461346453262,1.82896083721171,-2.76210933718279));
#7088=CARTESIAN_POINT('Ctrl Pts',(4.23132485355215,1.79998994807284,-2.75765383752922));
#7089=CARTESIAN_POINT('Ctrl Pts',(4.16963103391141,1.76773558300649,-2.75319833787564));
#7090=CARTESIAN_POINT('Ctrl Pts',(4.10802946459828,1.73552944766171,-2.74874950049886));
#7091=CARTESIAN_POINT('Ctrl Pts',(4.04801838350661,1.70004980615064,-2.74430066312208));
#7092=CARTESIAN_POINT('Ctrl Pts',(3.98996532425878,1.66148024969673,-2.7398518257453));
#7093=CARTESIAN_POINT('Ctrl Pts',(3.931980212784,1.62295583669438,-2.73540819547726));
#7094=CARTESIAN_POINT('Ctrl Pts',(3.87594897684726,1.58134896129237,-2.73096456520922));
#7095=CARTESIAN_POINT('Ctrl Pts',(3.82221350513018,1.53688850825699,-2.72652093494118));
#7096=CARTESIAN_POINT('Ctrl Pts',(3.76851163366005,1.49245585589319,-2.72208008323021));
#7097=CARTESIAN_POINT('Ctrl Pts',(3.71710305459827,1.44517347682411,-2.71763923151923));
#7098=CARTESIAN_POINT('Ctrl Pts',(3.66829842272948,1.39531193454344,-2.71319837980825));
#7099=CARTESIAN_POINT('Ctrl Pts',(3.6195077558972,1.34546465972534,-2.70875879880979));
#7100=CARTESIAN_POINT('Ctrl Pts',(3.57331989904164,1.29304003624274,-2.70431921781132));
#7101=CARTESIAN_POINT('Ctrl Pts',(3.53000901333487,1.23834582442945,-2.69987963681286));
#7102=CARTESIAN_POINT('Ctrl Pts',(3.486695832328,1.18364871404625,-2.69543982053472));
#7103=CARTESIAN_POINT('Ctrl Pts',(3.44626022694456,1.12668216153398,-2.69100000425659));
#7104=CARTESIAN_POINT('Ctrl Pts',(3.40893526309196,1.06778596804588,-2.68656018797846));
#7105=CARTESIAN_POINT('Ctrl Pts',(3.37157089991985,1.00882760517551,-2.68211568513879));
#7106=CARTESIAN_POINT('Ctrl Pts',(3.33732399411704,0.947935949964705,-2.67767118229911));
#7107=CARTESIAN_POINT('Ctrl Pts',(3.30638301824751,0.885477847757544,-2.67322667945944));
#7108=CARTESIAN_POINT('Ctrl Pts',(3.27542389170962,0.822983106230917,-2.66877956937501));
#7109=CARTESIAN_POINT('Ctrl Pts',(3.24777474903842,0.758920537938394,-2.66433245929058));
#7110=CARTESIAN_POINT('Ctrl Pts',(3.22357588420632,0.693676974462737,-2.65988534920616));
#7111=CARTESIAN_POINT('Ctrl Pts',(3.19933523994645,0.628320767738441,-2.65543056117006));
#7112=CARTESIAN_POINT('Ctrl Pts',(3.17855690974961,0.561779962659622,-2.65097577313396));
#7113=CARTESIAN_POINT('Ctrl Pts',(3.16133108332908,0.494455755073375,-2.64652098509787));
#7114=CARTESIAN_POINT('Ctrl Pts',(3.1525876784805,0.460283646945397,-2.64425984450796));
#7115=CARTESIAN_POINT('Ctrl Pts',(3.1447586939971,0.425909860714845,-2.64199870391805));
#7116=CARTESIAN_POINT('Ctrl Pts',(3.13785082285429,0.391387466346655,-2.63973756332814));
#7117=CARTESIAN_POINT('Ctrl Pts',(3.12423910047957,0.323362276221473,-2.63528206360562));
#7118=CARTESIAN_POINT('Ctrl Pts',(3.11415354892744,0.254492525885905,-2.6308265638831));
#7119=CARTESIAN_POINT('Ctrl Pts',(3.10769090350001,0.185176540570627,-2.62637106416058));
#7120=CARTESIAN_POINT('Ctrl Pts',(3.10123792161815,0.115964202931781,-2.62192222671359));
#7121=CARTESIAN_POINT('Ctrl Pts',(3.09839713858282,0.046307437830558,-2.61747338926661));
#7122=CARTESIAN_POINT('Ctrl Pts',(3.09921424000532,-0.0233854661888446,
-2.61302455181963));
#7123=CARTESIAN_POINT('Ctrl Pts',(3.1000303850578,-0.0929967986895868,-2.60858092147991));
#7124=CARTESIAN_POINT('Ctrl Pts',(3.10449590537496,-0.162643699280447,-2.6041372911402));
#7125=CARTESIAN_POINT('Ctrl Pts',(3.11260452902494,-0.231914783981276,-2.59969366080048));
#7126=CARTESIAN_POINT('Ctrl Pts',(3.12070808243626,-0.301142554187889,-2.59525280901695));
#7127=CARTESIAN_POINT('Ctrl Pts',(3.13245016324974,-0.36999448994615,-2.59081195723341));
#7128=CARTESIAN_POINT('Ctrl Pts',(3.14777253806218,-0.43806276791281,-2.58637110544988));
#7129=CARTESIAN_POINT('Ctrl Pts',(3.16309052850817,-0.506111568724173,-2.58193152437808));
#7130=CARTESIAN_POINT('Ctrl Pts',(3.18198667173287,-0.573376679921284,-2.57749194330629));
#7131=CARTESIAN_POINT('Ctrl Pts',(3.20435167568506,-0.639460689843633,-2.57305236223449));
#7132=CARTESIAN_POINT('Ctrl Pts',(3.2267178648945,-0.705548201958608,-2.56861254588236));
#7133=CARTESIAN_POINT('Ctrl Pts',(3.25255312069787,-0.770454025956134,-2.56417272953023));
#7134=CARTESIAN_POINT('Ctrl Pts',(3.28169891876835,-0.833797826999921,-2.5597329131781));
#7135=CARTESIAN_POINT('Ctrl Pts',(3.31087548243368,-0.897208492217892,-2.55528841026392));
#7136=CARTESIAN_POINT('Ctrl Pts',(3.34336935812326,-0.959053398371881,-2.55084390734974));
#7137=CARTESIAN_POINT('Ctrl Pts',(3.3789750817013,-1.01897493965707,-2.54639940443556));
#7138=CARTESIAN_POINT('Ctrl Pts',(3.41460169239576,-1.07893163226298,-2.54195229427624));
#7139=CARTESIAN_POINT('Ctrl Pts',(3.45334351273831,-1.13696230731877,-2.53750518411691));
#7140=CARTESIAN_POINT('Ctrl Pts',(3.49495211405337,-1.19273893392016,-2.53305807395759));
#7141=CARTESIAN_POINT('Ctrl Pts',(3.53663255276655,-1.24861185906569,-2.52860328584677));
#7142=CARTESIAN_POINT('Ctrl Pts',(3.58118933945791,-1.3022225916835,-2.52414849773595));
#7143=CARTESIAN_POINT('Ctrl Pts',(3.6283347529994,-1.35327734808887,-2.51969370962512));
#7144=CARTESIAN_POINT('Ctrl Pts',(3.65226459537614,-1.3791914759242,-2.51743256969006));
#7145=CARTESIAN_POINT('Ctrl Pts',(3.67686077852925,-1.4044477074082,-2.51517142975499));
#7146=CARTESIAN_POINT('Ctrl Pts',(3.70208239602594,-1.42901157696745,-2.51291028981993));
#7147=CARTESIAN_POINT('Ctrl Pts',(3.75178073939385,-1.47741385029353,-2.50845479013159));
#7148=CARTESIAN_POINT('Ctrl Pts',(3.80410472858639,-1.5233154944615,-2.50399929044326));
#7149=CARTESIAN_POINT('Ctrl Pts',(3.8587726100201,-1.56641879211955,-2.49954379075493));
#7150=CARTESIAN_POINT('Ctrl Pts',(3.91335874697203,-1.60945763773304,-2.49509495334257));
#7151=CARTESIAN_POINT('Ctrl Pts',(3.97028143874275,-1.64970614153343,-2.49064611593021));
#7152=CARTESIAN_POINT('Ctrl Pts',(4.02922281934548,-1.68690401921414,-2.48619727851785));
#7153=CARTESIAN_POINT('Ctrl Pts',(4.08809521245999,-1.72405835892337,-2.48175364821323));
#7154=CARTESIAN_POINT('Ctrl Pts',(4.14898118984444,-1.75816890447243,-2.4773100179086));
#7155=CARTESIAN_POINT('Ctrl Pts',(4.21153204421828,-1.78901729985797,-2.47286638760397));
#7156=CARTESIAN_POINT('Ctrl Pts',(4.27404378618446,-1.8198464060583,-2.4684255358558));
#7157=CARTESIAN_POINT('Ctrl Pts',(4.33821790217517,-1.84741719284653,-2.46398468410762));
#7158=CARTESIAN_POINT('Ctrl Pts',(4.40368042830157,-1.87155685393258,-2.45954383235944));
#7159=CARTESIAN_POINT('Ctrl Pts',(4.4691242228829,-1.89568960765993,-2.45510425132322));
#7160=CARTESIAN_POINT('Ctrl Pts',(4.53585523696321,-1.91639301563523,-2.450664670287));
#7161=CARTESIAN_POINT('Ctrl Pts',(4.60348049127541,-1.93354278758703,-2.44622508925078));
#7162=CARTESIAN_POINT('Ctrl Pts',(4.67110932945783,-1.9506934684087,-2.44178527293437));
#7163=CARTESIAN_POINT('Ctrl Pts',(4.73963202720664,-1.96429002141534,-2.43734545661797));
#7164=CARTESIAN_POINT('Ctrl Pts',(4.80864317708997,-1.97425876241818,-2.43290564030157));
#7165=CARTESIAN_POINT('Ctrl Pts',(4.87772717346325,-1.98423802618137,-2.42846113742313));
#7166=CARTESIAN_POINT('Ctrl Pts',(4.94730016595045,-1.99058176482097,-2.4240166345447));
#7167=CARTESIAN_POINT('Ctrl Pts',(5.01695030931486,-1.99326804846409,-2.41957213166627));
#7168=CARTESIAN_POINT('Ctrl Pts',(5.08664131101592,-1.99595590794145,-2.41512502154273));
#7169=CARTESIAN_POINT('Ctrl Pts',(5.15640906443546,-1.99498204875988,-2.4106779114192));
#7170=CARTESIAN_POINT('Ctrl Pts',(5.22584319353913,-1.99037667997494,-2.40623080129567));
#7171=CARTESIAN_POINT('Ctrl Pts',(5.29539720091904,-1.98576336000406,-2.40177601322035));
#7172=CARTESIAN_POINT('Ctrl Pts',(5.36461594863852,-1.97750607333603,-2.39732122514503));
#7173=CARTESIAN_POINT('Ctrl Pts',(5.43309644768473,-1.96568662554555,-2.39286643706971));
#7174=CARTESIAN_POINT('Ctrl Pts',(5.46785545536319,-1.95968736616184,-2.39060529681704));
#7175=CARTESIAN_POINT('Ctrl Pts',(5.50242446312932,-1.95277118902458,-2.38834415656438));
#7176=CARTESIAN_POINT('Ctrl Pts',(5.53675230609656,-1.94495369441729,-2.38608301631171));
#7177=CARTESIAN_POINT('Ctrl Pts',(5.60439414895831,-1.92954958812657,-2.38162751662287));
#7178=CARTESIAN_POINT('Ctrl Pts',(5.67136432185437,-1.91058233412087,-2.37717201693402));
#7179=CARTESIAN_POINT('Ctrl Pts',(5.73725977785801,-1.88812659081036,-2.37271651724518));
#7180=CARTESIAN_POINT('Ctrl Pts',(5.80305670086891,-1.86570442540835,-2.36826767983239));
#7181=CARTESIAN_POINT('Ctrl Pts',(5.86778163730379,-1.83980428061653,-2.3638188424196));
#7182=CARTESIAN_POINT('Ctrl Pts',(5.93104332991556,-1.81055147392126,-2.3593700050068));
#7183=CARTESIAN_POINT('Ctrl Pts',(5.99423097836069,-1.78133290595096,-2.3549263747019));
#7184=CARTESIAN_POINT('Ctrl Pts',(6.05595834269379,-1.74876967434823,-2.350482744397));
#7185=CARTESIAN_POINT('Ctrl Pts',(6.11585259374666,-1.71303577486895,-2.3460391140921));
#7186=CARTESIAN_POINT('Ctrl Pts',(6.17570939353755,-1.67732421943117,-2.34159826234373));
#7187=CARTESIAN_POINT('Ctrl Pts',(6.23373493485255,-1.63844617932036,-2.33715741059537));
#7188=CARTESIAN_POINT('Ctrl Pts',(6.28958089198515,-1.59662160954613,-2.332716558847));
#7189=CARTESIAN_POINT('Ctrl Pts',(6.3454108692708,-1.55480900751777,-2.32827697781069));
#7190=CARTESIAN_POINT('Ctrl Pts',(6.39906210918047,-1.51005184274183,-2.32383739677439));
#7191=CARTESIAN_POINT('Ctrl Pts',(6.45021667187041,-1.46261240328846,-2.31939781573808));
#7192=CARTESIAN_POINT('Ctrl Pts',(6.50137394554798,-1.41517044973417,-2.3149579994217));
#7193=CARTESIAN_POINT('Ctrl Pts',(6.5500339222949,-1.36504627368842,-2.31051818310532));
#7194=CARTESIAN_POINT('Ctrl Pts',(6.59591438312211,-1.31254010337729,-2.30607836678895));
#7195=CARTESIAN_POINT('Ctrl Pts',(6.64184327424584,-1.25997850883215,-2.30163386391064));
#7196=CARTESIAN_POINT('Ctrl Pts',(6.6849864710863,-1.2050302707258,-2.29718936103235));
#7197=CARTESIAN_POINT('Ctrl Pts',(6.72510169553051,-1.14802915354762,-2.29274485815405));
#7198=CARTESIAN_POINT('Ctrl Pts',(6.76524045246458,-1.0909945982364,-2.28829774803073));
#7199=CARTESIAN_POINT('Ctrl Pts',(6.80234744129299,-1.03190518124544,-2.28385063790742));
#7200=CARTESIAN_POINT('Ctrl Pts',(6.83622494570269,-0.971121775594272,-2.2794035277841));
#7201=CARTESIAN_POINT('Ctrl Pts',(6.87016093974603,-0.910233427173865,-2.27494873970911));
#7202=CARTESIAN_POINT('Ctrl Pts',(6.90085610448131,-0.847645691295311,-2.27049395163411));
#7203=CARTESIAN_POINT('Ctrl Pts',(6.92816004693264,-0.78374128750267,-2.26603916355912));
#7204=CARTESIAN_POINT('Ctrl Pts',(6.94201885284491,-0.751304992609359,-2.26377802330725));
#7205=CARTESIAN_POINT('Ctrl Pts',(6.95500475721979,-0.718529756660505,-2.26151688305537));
#7206=CARTESIAN_POINT('Ctrl Pts',(6.96710304201812,-0.685467005270186,-2.2592557428035));
#7207=CARTESIAN_POINT('Ctrl Pts',(6.99459284271437,-0.610341608460643,-2.25411796534938));
#7208=CARTESIAN_POINT('Ctrl Pts',(7.01758619456045,-0.533487851592203,-2.24898018789526));
#7209=CARTESIAN_POINT('Ctrl Pts',(7.03589429966574,-0.455414942519256,-2.24384241044115));
#7210=CARTESIAN_POINT('Ctrl Pts',(7.05404569288441,-0.378010314123302,-2.23874861082052));
#7211=CARTESIAN_POINT('Ctrl Pts',(7.06759161076418,-0.299407491567439,-2.2336548111999));
#7212=CARTESIAN_POINT('Ctrl Pts',(7.07639445970045,-0.220123707558807,-2.22856101157927));
#7213=CARTESIAN_POINT('Ctrl Pts',(7.08444110624045,-0.147650739899122,-2.22390479114546));
#7214=CARTESIAN_POINT('Ctrl Pts',(7.08852500633563,-0.074609111606327,-2.21924857071165));
#7215=CARTESIAN_POINT('Ctrl Pts',(7.08857665886015,-0.00140753592614233,
-2.21459235027785));
#7216=CARTESIAN_POINT('Ctrl Pts',(7.08857715545311,1.10874632379271E-10,
-3.17330009074087));
#7217=CARTESIAN_POINT('Ctrl Pts',(7.08857715545308,0.000599462197711708,
-3.17325859730295));
#7218=CARTESIAN_POINT('Ctrl Pts',(7.08857688524422,0.0011989297675538,-3.17321709980395));
#7219=CARTESIAN_POINT('Ctrl Pts',(7.08855819985703,0.0219243629936726,-3.17178227682757));
#7220=CARTESIAN_POINT('Ctrl Pts',(7.08823546589232,0.0420486590280136,-3.17038492010015));
#7221=CARTESIAN_POINT('Ctrl Pts',(7.08334010096522,0.199056332811374,-3.15945848135308));
#7222=CARTESIAN_POINT('Ctrl Pts',(7.06498484703654,0.335153782962829,-3.14981256578896));
#7223=CARTESIAN_POINT('Ctrl Pts',(7.02925382032359,0.483097077674355,-3.13973835663072));
#7224=CARTESIAN_POINT('Ctrl Pts',(7.02551172499111,0.497849293242752,-3.1387388094495));
#7225=CARTESIAN_POINT('Ctrl Pts',(7.02008490974601,0.51826001278871,-3.13736418295022));
#7226=CARTESIAN_POINT('Ctrl Pts',(7.01854347430543,0.523955600119139,-3.13698149880969));
#7227=CARTESIAN_POINT('Ctrl Pts',(7.01584851381334,0.533741057508895,-3.13632567385635));
#7228=CARTESIAN_POINT('Ctrl Pts',(7.01470716129347,0.53783419605856,-3.13605185003928));
#7229=CARTESIAN_POINT('Ctrl Pts',(7.01228917827564,0.546399726230936,-3.13547992441716));
#7230=CARTESIAN_POINT('Ctrl Pts',(7.01100997372563,0.550871342282968,-3.13518198267385));
#7231=CARTESIAN_POINT('Ctrl Pts',(7.00784178879654,0.561801410411964,-3.13445517294403));
#7232=CARTESIAN_POINT('Ctrl Pts',(7.00593572353959,0.568254932546007,-3.13402728285012));
#7233=CARTESIAN_POINT('Ctrl Pts',(6.99892426319377,0.591559453513844,-3.13248621205023));
#7234=CARTESIAN_POINT('Ctrl Pts',(6.99362829990496,0.608352889783915,-3.13138346980831));
#7235=CARTESIAN_POINT('Ctrl Pts',(6.97984408802542,0.650125823019246,-3.12865480406176));
#7236=CARTESIAN_POINT('Ctrl Pts',(6.97108119055639,0.675011761329208,-3.12704216521398));
#7237=CARTESIAN_POINT('Ctrl Pts',(6.93081149283235,0.782517659410478,-3.1201027036711));
#7238=CARTESIAN_POINT('Ctrl Pts',(6.89432279725226,0.863170427002166,-3.11496381255671));
#7239=CARTESIAN_POINT('Ctrl Pts',(6.78401015454395,1.06931903808697,-3.10138862513449));
#7240=CARTESIAN_POINT('Ctrl Pts',(6.7016233009776,1.18959966672738,-3.0929708270439));
#7241=CARTESIAN_POINT('Ctrl Pts',(6.59069505190685,1.31872392252539,-3.08249444309442));
#7242=CARTESIAN_POINT('Ctrl Pts',(6.57413522328348,1.33728614082925,-3.08095037489573));
#7243=CARTESIAN_POINT('Ctrl Pts',(6.5505292194155,1.36277070092467,-3.07877380360066));
#7244=CARTESIAN_POINT('Ctrl Pts',(6.54377175695719,1.36995822324756,-3.07815344641891));
#7245=CARTESIAN_POINT('Ctrl Pts',(6.53129710752092,1.383031097873,-3.07701297483722));
#7246=CARTESIAN_POINT('Ctrl Pts',(6.5255963636265,1.38893189611541,-3.07649357206908));
#7247=CARTESIAN_POINT('Ctrl Pts',(6.51396563835607,1.40082307913303,-3.07543735871395));
#7248=CARTESIAN_POINT('Ctrl Pts',(6.50803377187297,1.40681137760315,-3.07490047142813));
#7249=CARTESIAN_POINT('Ctrl Pts',(6.49327891846793,1.42151897432977,-3.07356932572655));
#7250=CARTESIAN_POINT('Ctrl Pts',(6.48441230790119,1.4301938168302,-3.07277314627218));
#7251=CARTESIAN_POINT('Ctrl Pts',(6.45081512391981,1.46245655996554,-3.06976973918098));
#7252=CARTESIAN_POINT('Ctrl Pts',(6.42556181110556,1.48548918045345,-3.06753906195773));
#7253=CARTESIAN_POINT('Ctrl Pts',(6.36051183122157,1.54182660836251,-3.06185559227363));
#7254=CARTESIAN_POINT('Ctrl Pts',(6.31998585893191,1.57424694483761,-3.05837030204562));
#7255=CARTESIAN_POINT('Ctrl Pts',(6.18634616739285,1.6728640373679,-3.04705977449551));
#7256=CARTESIAN_POINT('Ctrl Pts',(6.08879785467727,1.73265736179203,-3.03905845787811));
#7257=CARTESIAN_POINT('Ctrl Pts',(5.90555242892172,1.82437944775786,-3.02480992475655));
#7258=CARTESIAN_POINT('Ctrl Pts',(5.82173868182922,1.859410380186,-3.01856146136709));
#7259=CARTESIAN_POINT('Ctrl Pts',(5.72545309783015,1.89214063303886,-3.01187724978873));
#7260=CARTESIAN_POINT('Ctrl Pts',(5.71505479225973,1.89558005436162,-3.01116172138711));
#7261=CARTESIAN_POINT('Ctrl Pts',(5.69926637141212,1.90065847653283,-3.0100854003819));
#7262=CARTESIAN_POINT('Ctrl Pts',(5.69389697192569,1.90236050891383,-3.00972112165501));
#7263=CARTESIAN_POINT('Ctrl Pts',(5.68422790960847,1.90538046974482,-3.00906839323145));
#7264=CARTESIAN_POINT('Ctrl Pts',(5.67993095539784,1.90670661662102,-3.00877947755593));
#7265=CARTESIAN_POINT('Ctrl Pts',(5.67048094406062,1.90958816028564,-3.00814662882166));
#7266=CARTESIAN_POINT('Ctrl Pts',(5.66532606828273,1.91113723423796,-3.00780306265572));
#7267=CARTESIAN_POINT('Ctrl Pts',(5.65048309252642,1.91553222010498,-3.00681835513865));
#7268=CARTESIAN_POINT('Ctrl Pts',(5.64077940472971,1.91832551086783,-3.00618016772019));
#7269=CARTESIAN_POINT('Ctrl Pts',(5.57026564435231,1.93804495109615,-3.00158015395771));
#7270=CARTESIAN_POINT('Ctrl Pts',(5.50869716520569,1.95215175051466,-2.9977649488736));
#7271=CARTESIAN_POINT('Ctrl Pts',(5.31807572058205,1.98639886348312,-2.98627866568773));
#7272=CARTESIAN_POINT('Ctrl Pts',(5.18763569593124,1.99681510417929,-2.97884991967218));
#7273=CARTESIAN_POINT('Ctrl Pts',(4.96779674576504,1.99276773575839,-2.96591712762864));
#7274=CARTESIAN_POINT('Ctrl Pts',(4.87870633027246,1.98512645102287,-2.96056572148074));
#7275=CARTESIAN_POINT('Ctrl Pts',(4.77494547054984,1.96915911626876,-2.95405053549089));
#7276=CARTESIAN_POINT('Ctrl Pts',(4.75948541340779,1.96659317904938,-2.95307251956547));
#7277=CARTESIAN_POINT('Ctrl Pts',(4.7341602256607,1.96208265015669,-2.9514577364435));
#7278=CARTESIAN_POINT('Ctrl Pts',(4.72427653730745,1.96024512781647,-2.95082434648351));
#7279=CARTESIAN_POINT('Ctrl Pts',(4.70651566754514,1.95680402430243,-2.94968022908205));
#7280=CARTESIAN_POINT('Ctrl Pts',(4.69863344113995,1.95522737892046,-2.94917036554373));
#7281=CARTESIAN_POINT('Ctrl Pts',(4.68183011782371,1.95176052843171,-2.9480788396038));
#7282=CARTESIAN_POINT('Ctrl Pts',(4.67291204795625,1.94985670937686,-2.94749675445292));
#7283=CARTESIAN_POINT('Ctrl Pts',(4.64878571595056,1.94453301924304,-2.94591433253504));
#7284=CARTESIAN_POINT('Ctrl Pts',(4.6336042300655,1.94099597679873,-2.94491028469131));
#7285=CARTESIAN_POINT('Ctrl Pts',(4.55305830992402,1.92123199614168,-2.93953776417323));
#7286=CARTESIAN_POINT('Ctrl Pts',(4.48851241563625,1.90188213171461,-2.93507014459762));
#7287=CARTESIAN_POINT('Ctrl Pts',(4.27204102409429,1.82485063381894,-2.9195228906552));
#7288=CARTESIAN_POINT('Ctrl Pts',(4.12623744836733,1.75190534748897,-2.9080144945353));
#7289=CARTESIAN_POINT('Ctrl Pts',(3.94415105596452,1.63108013443148,-2.89301170889262));
#7290=CARTESIAN_POINT('Ctrl Pts',(3.89871125274439,1.59808534164191,-2.88921488632742));
#7291=CARTESIAN_POINT('Ctrl Pts',(3.84741261208193,1.55742264339405,-2.88491815662332));
#7292=CARTESIAN_POINT('Ctrl Pts',(3.84014606263841,1.55157926952471,-2.88430927925407));
#7293=CARTESIAN_POINT('Ctrl Pts',(3.82844597196557,1.54203481452343,-2.88332888610201));
#7294=CARTESIAN_POINT('Ctrl Pts',(3.82398715849579,1.53836513639445,-2.88295526090424));
#7295=CARTESIAN_POINT('Ctrl Pts',(3.81607763090086,1.53179764267695,-2.88229257161583));
#7296=CARTESIAN_POINT('Ctrl Pts',(3.8126207405265,1.52890744956191,-2.88200297619616));
#7297=CARTESIAN_POINT('Ctrl Pts',(3.80514065358463,1.52261040757635,-2.8813764347959));
#7298=CARTESIAN_POINT('Ctrl Pts',(3.80112116155103,1.51919931813778,-2.8810398025404));
#7299=CARTESIAN_POINT('Ctrl Pts',(3.78983648953625,1.50954551365542,-2.88009468474169));
#7300=CARTESIAN_POINT('Ctrl Pts',(3.78260256871981,1.50326624601553,-2.87948879500414));
#7301=CARTESIAN_POINT('Ctrl Pts',(3.73748717842351,1.46353123690688,-2.87570779775224));
#7302=CARTESIAN_POINT('Ctrl Pts',(3.70083994449417,1.42869499687468,-2.87262618803146));
#7303=CARTESIAN_POINT('Ctrl Pts',(3.59548929689736,1.32063787629418,-2.86359261399795));
#7304=CARTESIAN_POINT('Ctrl Pts',(3.53094533123544,1.24358499474055,-2.85781284671031));
#7305=CARTESIAN_POINT('Ctrl Pts',(3.39557524041277,1.05470074869476,-2.8443091295812));
#7306=CARTESIAN_POINT('Ctrl Pts',(3.32952882804349,0.940052181009512,-2.83656388734938));
#7307=CARTESIAN_POINT('Ctrl Pts',(3.26863874945042,0.804970158107974,-2.82737491614366));
#7308=CARTESIAN_POINT('Ctrl Pts',(3.26216573805277,0.790130432826794,-2.8263650863912));
#7309=CARTESIAN_POINT('Ctrl Pts',(3.25190633900863,0.765806445899519,-2.82470847652323));
#7310=CARTESIAN_POINT('Ctrl Pts',(3.24801080184816,0.756368818228067,-2.82406538305793));
#7311=CARTESIAN_POINT('Ctrl Pts',(3.2411724132598,0.739434127479379,-2.82291064384033));
#7312=CARTESIAN_POINT('Ctrl Pts',(3.23820216995446,0.73194831289552,-2.82239993067219));
#7313=CARTESIAN_POINT('Ctrl Pts',(3.23200145828401,0.716040501512925,-2.82131396231731));
#7314=CARTESIAN_POINT('Ctrl Pts',(3.22878263051223,0.707614190108583,-2.82073833197637));
#7315=CARTESIAN_POINT('Ctrl Pts',(3.2203156685789,0.684990064607807,-2.81919159130164));
#7316=CARTESIAN_POINT('Ctrl Pts',(3.21517188729456,0.670754085046129,-2.81821705028842));
#7317=CARTESIAN_POINT('Ctrl Pts',(3.19013611969438,0.598916969227695,-2.81329195112207));
#7318=CARTESIAN_POINT('Ctrl Pts',(3.17273091629326,0.540489618055237,-2.80926097638077));
#7319=CARTESIAN_POINT('Ctrl Pts',(3.12687276047993,0.356070950706149,-2.79645435599716));
#7320=CARTESIAN_POINT('Ctrl Pts',(3.10795783213181,0.22806195218001,-2.78742380415097));
#7321=CARTESIAN_POINT('Ctrl Pts',(3.09680022457168,0.00384556538273569,
-2.77180067554752));
#7322=CARTESIAN_POINT('Ctrl Pts',(3.09890096906112,-0.0916795623901858,
-2.76521469552477));
#7323=CARTESIAN_POINT('Ctrl Pts',(3.10885811464207,-0.197599032530022,-2.75822224834573));
#7324=CARTESIAN_POINT('Ctrl Pts',(3.10997277672483,-0.208492895744148,-2.75750682781076));
#7325=CARTESIAN_POINT('Ctrl Pts',(3.11179654074277,-0.224975391926986,-2.75643063690742));
#7326=CARTESIAN_POINT('Ctrl Pts',(3.11243967545514,-0.23057090147684,-2.75606638162384));
#7327=CARTESIAN_POINT('Ctrl Pts',(3.11363891316854,-0.240628988111074,-2.75541367810742));
#7328=CARTESIAN_POINT('Ctrl Pts',(3.11418641163659,-0.245092454812895,-2.75512476405867));
#7329=CARTESIAN_POINT('Ctrl Pts',(3.11542243430872,-0.254894676855335,-2.7544918986872));
#7330=CARTESIAN_POINT('Ctrl Pts',(3.11611747457295,-0.260232505130362,-2.75414831439715));
#7331=CARTESIAN_POINT('Ctrl Pts',(3.11817859553243,-0.275576330403442,-2.75316350253923));
#7332=CARTESIAN_POINT('Ctrl Pts',(3.11959908821063,-0.285575024830621,-2.75252522987678));
#7333=CARTESIAN_POINT('Ctrl Pts',(3.13045409874494,-0.358026723464336,-2.74792264118044));
#7334=CARTESIAN_POINT('Ctrl Pts',(3.14277524680914,-0.420017931764002,-2.74410513326315));
#7335=CARTESIAN_POINT('Ctrl Pts',(3.18957166695359,-0.608224869583766,-2.73260349136378));
#7336=CARTESIAN_POINT('Ctrl Pts',(3.23352617170598,-0.731716781852988,-2.72516246728735));
#7337=CARTESIAN_POINT('Ctrl Pts',(3.32721120771476,-0.930607595809442,-2.71222973258471));
#7338=CARTESIAN_POINT('Ctrl Pts',(3.37052061051785,-1.00855047430586,-2.70689262587135));
#7339=CARTESIAN_POINT('Ctrl Pts',(3.42739549837876,-1.09648457176304,-2.70039337637139));
#7340=CARTESIAN_POINT('Ctrl Pts',(3.43605621509267,-1.10953520509804,-2.69941589002208));
#7341=CARTESIAN_POINT('Ctrl Pts',(3.45052509481402,-1.13079039226603,-2.69780180355726));
#7342=CARTESIAN_POINT('Ctrl Pts',(3.45624328259062,-1.13905558563002,-2.69716857562696));
#7343=CARTESIAN_POINT('Ctrl Pts',(3.46664674010609,-1.15385270745091,-2.69602463369584));
#7344=CARTESIAN_POINT('Ctrl Pts',(3.47130952444587,-1.16040023637221,-2.69551478244949));
#7345=CARTESIAN_POINT('Ctrl Pts',(3.48134732194818,-1.17431662592668,-2.69442315499969));
#7346=CARTESIAN_POINT('Ctrl Pts',(3.48673354148419,-1.18167713982591,-2.69384095521477));
#7347=CARTESIAN_POINT('Ctrl Pts',(3.50146616940529,-1.20152290279843,-2.69225789936058));
#7348=CARTESIAN_POINT('Ctrl Pts',(3.51090867614908,-1.21393569058628,-2.6912533271544));
#7349=CARTESIAN_POINT('Ctrl Pts',(3.5619713908644,-1.27945209224144,-2.68587234365543));
#7350=CARTESIAN_POINT('Ctrl Pts',(3.60611588380436,-1.3305236385502,-2.68139641038207));
#7351=CARTESIAN_POINT('Ctrl Pts',(3.76562628947781,-1.49718260190214,-2.66578553157318));
#7352=CARTESIAN_POINT('Ctrl Pts',(3.89254069301763,-1.6008041593079,-2.65421694403471));
#7353=CARTESIAN_POINT('Ctrl Pts',(4.07738317138215,-1.71724266913717,-2.63922608057721));
#7354=CARTESIAN_POINT('Ctrl Pts',(4.12534429680093,-1.74474150023,-2.63548991167286));
#7355=CARTESIAN_POINT('Ctrl Pts',(4.18263260946149,-1.77449664234036,-2.63125291024725));
#7356=CARTESIAN_POINT('Ctrl Pts',(4.1909053520917,-1.77872034318595,-2.63064641760298));
#7357=CARTESIAN_POINT('Ctrl Pts',(4.20435913868881,-1.78547120712331,-2.6296690978502));
#7358=CARTESIAN_POINT('Ctrl Pts',(4.20952205228512,-1.78803391210372,-2.62929618221603));
#7359=CARTESIAN_POINT('Ctrl Pts',(4.2187399988187,-1.79255971342181,-2.62863426021949));
#7360=CARTESIAN_POINT('Ctrl Pts',(4.22279064027287,-1.79453148439082,-2.62834472746863));
#7361=CARTESIAN_POINT('Ctrl Pts',(4.23160281608187,-1.79878420722699,-2.62771775740988));
#7362=CARTESIAN_POINT('Ctrl Pts',(4.23636673380252,-1.80105998301711,-2.62738063762035));
#7363=CARTESIAN_POINT('Ctrl Pts',(4.24983185105195,-1.80742688221737,-2.62643275574421));
#7364=CARTESIAN_POINT('Ctrl Pts',(4.25855381394333,-1.81147411301936,-2.62582461376662));
#7365=CARTESIAN_POINT('Ctrl Pts',(4.3139814206665,-1.83670859642773,-2.62199467609262));
#7366=CARTESIAN_POINT('Ctrl Pts',(4.36146461431275,-1.85615299318411,-2.61886920120932));
#7367=CARTESIAN_POINT('Ctrl Pts',(4.55391893185157,-1.92642559753121,-2.60661253281853));
#7368=CARTESIAN_POINT('Ctrl Pts',(4.70379578034513,-1.96226856984545,-2.5979392534222));
#7369=CARTESIAN_POINT('Ctrl Pts',(4.93545402025679,-1.99005012829157,-2.58415291208009));
#7370=CARTESIAN_POINT('Ctrl Pts',(5.0150882535075,-1.99478809674902,-2.57935517585511));
#7371=CARTESIAN_POINT('Ctrl Pts',(5.11008303245937,-1.99474241310027,-2.57345672839195));
#7372=CARTESIAN_POINT('Ctrl Pts',(5.1253786860223,-1.99455910636388,-2.57250172253999));
#7373=CARTESIAN_POINT('Ctrl Pts',(5.15060636511678,-1.99396651472431,-2.57091723461746));
#7374=CARTESIAN_POINT('Ctrl Pts',(5.1605403054555,-1.99365887011127,-2.57029091349595));
#7375=CARTESIAN_POINT('Ctrl Pts',(5.17849470039393,-1.9929684990042,-2.56915440867983));
#7376=CARTESIAN_POINT('Ctrl Pts',(5.18651597785913,-1.99261155530148,-2.56864503884174));
#7377=CARTESIAN_POINT('Ctrl Pts',(5.20372150112516,-1.99174180220805,-2.56754886083598));
#7378=CARTESIAN_POINT('Ctrl Pts',(5.21290476363112,-1.99121387410926,-2.56696159251266));
#7379=CARTESIAN_POINT('Ctrl Pts',(5.23800282211048,-1.98959679408237,-2.56535041177679));
#7380=CARTESIAN_POINT('Ctrl Pts',(5.25390845052865,-1.98838024039937,-2.56432255550063));
#7381=CARTESIAN_POINT('Ctrl Pts',(5.34271759863926,-1.98051512736598,-2.55854423134054));
#7382=CARTESIAN_POINT('Ctrl Pts',(5.41521838799733,-1.97004874809723,-2.55367573803175));
#7383=CARTESIAN_POINT('Ctrl Pts',(5.58306179456705,-1.93630658823773,-2.54205108104042));
#7384=CARTESIAN_POINT('Ctrl Pts',(5.67758910638322,-1.90993530281414,-2.5352260734693));
#7385=CARTESIAN_POINT('Ctrl Pts',(5.86815384222339,-1.84129762540535,-2.52110583258603));
#7386=CARTESIAN_POINT('Ctrl Pts',(5.96359245790004,-1.79818558055694,-2.51383148247287));
#7387=CARTESIAN_POINT('Ctrl Pts',(6.06945908717783,-1.73995231235122,-2.5058220191991));
#7388=CARTESIAN_POINT('Ctrl Pts',(6.08360394316704,-1.73194505292132,-2.50475338193356));
#7389=CARTESIAN_POINT('Ctrl Pts',(6.10346738184406,-1.72037771904275,-2.50325652823694));
#7390=CARTESIAN_POINT('Ctrl Pts',(6.10926780035158,-1.71696044880687,-2.50281989183592));
#7391=CARTESIAN_POINT('Ctrl Pts',(6.11890370945152,-1.71121761841299,-2.50209545576842));
#7392=CARTESIAN_POINT('Ctrl Pts',(6.12274881544539,-1.70890839368137,-2.50180662423489));
#7393=CARTESIAN_POINT('Ctrl Pts',(6.13059990769312,-1.7041572206578,-2.5012174338885));
#7394=CARTESIAN_POINT('Ctrl Pts',(6.13460512208584,-1.70171407638988,-2.50091715561444));
#7395=CARTESIAN_POINT('Ctrl Pts',(6.14468431829071,-1.6955169624728,-2.50016214899386));
#7396=CARTESIAN_POINT('Ctrl Pts',(6.15074689275019,-1.69174443085517,-2.49970861472096));
#7397=CARTESIAN_POINT('Ctrl Pts',(6.16390253631906,-1.68345980287491,-2.49872546297339));
#7398=CARTESIAN_POINT('Ctrl Pts',(6.17098763765437,-1.67893523693992,-2.49819662000978));
#7399=CARTESIAN_POINT('Ctrl Pts',(6.19139450518203,-1.66572099835597,-2.49667464060269));
#7400=CARTESIAN_POINT('Ctrl Pts',(6.20464152324734,-1.65691641483263,-2.49568817162834));
#7401=CARTESIAN_POINT('Ctrl Pts',(6.25053053157035,-1.62561870653975,-2.49227101656605));
#7402=CARTESIAN_POINT('Ctrl Pts',(6.28260783228616,-1.60231075923823,-2.48988241958157));
#7403=CARTESIAN_POINT('Ctrl Pts',(6.38771542861098,-1.52104242085849,-2.48197949488714));
#7404=CARTESIAN_POINT('Ctrl Pts',(6.45737577984375,-1.45892211827249,-2.47660883735775));
#7405=CARTESIAN_POINT('Ctrl Pts',(6.61331371178524,-1.2989006158401,-2.46362201147581));
#7406=CARTESIAN_POINT('Ctrl Pts',(6.69482689403146,-1.1969860626194,-2.45597534774945));
#7407=CARTESIAN_POINT('Ctrl Pts',(6.77466215837702,-1.07428292892219,-2.44689708306991));
#7408=CARTESIAN_POINT('Ctrl Pts',(6.7833329776571,-1.06059425376905,-2.44588640953958));
#7409=CARTESIAN_POINT('Ctrl Pts',(6.79719604010469,-1.03810709182073,-2.44422869124023));
#7410=CARTESIAN_POINT('Ctrl Pts',(6.80248926118714,-1.02937150412238,-2.4435853414909));
#7411=CARTESIAN_POINT('Ctrl Pts',(6.81183584765462,-1.01367576831297,-2.44243031917921));
#7412=CARTESIAN_POINT('Ctrl Pts',(6.81591461598052,-1.0067309496303,-2.44191958101522));
#7413=CARTESIAN_POINT('Ctrl Pts',(6.82447082349166,-0.991958354125411,-2.44083374727074));
#7414=CARTESIAN_POINT('Ctrl Pts',(6.82893745106589,-0.984124554978757,-2.4402582777393));
#7415=CARTESIAN_POINT('Ctrl Pts',(6.84075334876596,-0.963070721916951,-2.43871242491866));
#7416=CARTESIAN_POINT('Ctrl Pts',(6.84800551274211,-0.949797141649947,-2.43773861781169));
#7417=CARTESIAN_POINT('Ctrl Pts',(6.88364374943014,-0.882768086197412,-2.43282397972328));
#7418=CARTESIAN_POINT('Ctrl Pts',(6.90971035575264,-0.827822346857297,-2.42880314442229));
#7419=CARTESIAN_POINT('Ctrl Pts',(7.00196426767203,-0.607950867054155,-2.41273593145567));
#7420=CARTESIAN_POINT('Ctrl Pts',(7.04849773362159,-0.435706415553922,-2.40010830636737));
#7421=CARTESIAN_POINT('Ctrl Pts',(7.07540191313661,-0.230730475128536,-2.38597561417028));
#7422=CARTESIAN_POINT('Ctrl Pts',(7.07855837344646,-0.201785105911168,-2.38400261190848));
#7423=CARTESIAN_POINT('Ctrl Pts',(7.08314538899354,-0.14902681609023,-2.380459073846));
#7424=CARTESIAN_POINT('Ctrl Pts',(7.08478463972377,-0.125237544368088,-2.37888063083536));
#7425=CARTESIAN_POINT('Ctrl Pts',(7.08639479754835,-0.0936106371364966,
-2.37681274808185));
#7426=CARTESIAN_POINT('Ctrl Pts',(7.08674659769538,-0.0857954621362452,
-2.37630424185497));
#7427=CARTESIAN_POINT('Ctrl Pts',(7.08724338861386,-0.0730968440859805,
-2.3754822302458));
#7428=CARTESIAN_POINT('Ctrl Pts',(7.08741642779279,-0.0682146736635013,
-2.37516721412269));
#7429=CARTESIAN_POINT('Ctrl Pts',(7.08770735024483,-0.0590561701382827,
-2.37457824453436));
#7430=CARTESIAN_POINT('Ctrl Pts',(7.08782941437726,-0.0547800525580501,
-2.37430406518427));
#7431=CARTESIAN_POINT('Ctrl Pts',(7.08805314365561,-0.0459461989416382,
-2.37373927019286));
#7432=CARTESIAN_POINT('Ctrl Pts',(7.08815294255975,-0.0413884172803767,
-2.37344875705754));
#7433=CARTESIAN_POINT('Ctrl Pts',(7.08834967083952,-0.0307353121714973,
-2.37277172434694));
#7434=CARTESIAN_POINT('Ctrl Pts',(7.08843428665534,-0.0246397686534487,
-2.37238586387929));
#7435=CARTESIAN_POINT('Ctrl Pts',(7.08854690723388,-0.0125257633651796,
-2.37162188786747));
#7436=CARTESIAN_POINT('Ctrl Pts',(7.08857562044022,-0.00650738880385826,
-2.37124374122592));
#7437=CARTESIAN_POINT('Ctrl Pts',(7.08857709553938,-0.000488902672746962,
-2.37086691085377));
#7438=CARTESIAN_POINT('Origin',(5.09382715545311,0.,-6.77268258743872));
#7439=CARTESIAN_POINT('',(7.08857715545311,-2.35333930719797E-11,-1.41355420449641));
#7440=CARTESIAN_POINT('',(7.08857715545311,2.4467182997506E-11,-1.57370881642439));
#7441=CARTESIAN_POINT('',(7.08857715545311,8.3550772080578E-14,-6.77268258743872));
#7442=CARTESIAN_POINT('Ctrl Pts',(7.08857715545311,-2.35333930719797E-11,
-1.41355420449641));
#7443=CARTESIAN_POINT('Ctrl Pts',(7.08857715545221,-0.0760979527884141,
-1.4180590646126));
#7444=CARTESIAN_POINT('Ctrl Pts',(7.08422265901158,-0.152126174664224,-1.42264720274503));
#7445=CARTESIAN_POINT('Ctrl Pts',(7.07380624441203,-0.242776045741805,-1.42831398992487));
#7446=CARTESIAN_POINT('Ctrl Pts',(7.07190396716427,-0.257816811514585,-1.42926063316788));
#7447=CARTESIAN_POINT('Ctrl Pts',(7.06847680026894,-0.282638095745051,-1.43083410243593));
#7448=CARTESIAN_POINT('Ctrl Pts',(7.06705020328532,-0.292431719854238,-1.43145784456551));
#7449=CARTESIAN_POINT('Ctrl Pts',(7.06433477461791,-0.310147880213191,-1.43259160122804));
#7450=CARTESIAN_POINT('Ctrl Pts',(7.06307088536315,-0.318074069881306,-1.43310082018308));
#7451=CARTESIAN_POINT('Ctrl Pts',(7.06025093570649,-0.335097382806626,-1.43419883612959));
#7452=CARTESIAN_POINT('Ctrl Pts',(7.05867951192604,-0.344191737359292,-1.43478810757055));
#7453=CARTESIAN_POINT('Ctrl Pts',(7.05419493901455,-0.369113400100443,-1.43641043444629));
#7454=CARTESIAN_POINT('Ctrl Pts',(7.05115332601244,-0.384916596047755,-1.43744752561958));
#7455=CARTESIAN_POINT('Ctrl Pts',(7.03271966714409,-0.474816311443012,-1.44339632336613));
#7456=CARTESIAN_POINT('Ctrl Pts',(7.01331380419635,-0.548017567586935,-1.44843453417937));
#7457=CARTESIAN_POINT('Ctrl Pts',(6.95485760376048,-0.726797243136719,-1.46122412816399));
#7458=CARTESIAN_POINT('Ctrl Pts',(6.91094536633002,-0.830509608792088,-1.46909053202858));
#7459=CARTESIAN_POINT('Ctrl Pts',(6.81398900352541,-1.0144956315532,-1.48356403772491));
#7460=CARTESIAN_POINT('Ctrl Pts',(6.76341905098709,-1.0957305166476,-1.49016014346713));
#7461=CARTESIAN_POINT('Ctrl Pts',(6.70077471425887,-1.18189128702913,-1.49716182494519));
#7462=CARTESIAN_POINT('Ctrl Pts',(6.69426228757446,-1.19069512131317,-1.4978772469108));
#7463=CARTESIAN_POINT('Ctrl Pts',(6.68429084513701,-1.20394540427319,-1.49895343953243));
#7464=CARTESIAN_POINT('Ctrl Pts',(6.68088507605155,-1.20843139781207,-1.49931769511946));
#7465=CARTESIAN_POINT('Ctrl Pts',(6.67472596013743,-1.21647307990937,-1.49997039890692));
#7466=CARTESIAN_POINT('Ctrl Pts',(6.67197956235814,-1.22003392024961,-1.5002593129258));
#7467=CARTESIAN_POINT('Ctrl Pts',(6.66591924104566,-1.22783672012552,-1.50089217789054));
#7468=CARTESIAN_POINT('Ctrl Pts',(6.6626001843452,-1.23207456037774,-1.50123576180621));
#7469=CARTESIAN_POINT('Ctrl Pts',(6.65300504670706,-1.24422419569824,-1.50222057185984));
#7470=CARTESIAN_POINT('Ctrl Pts',(6.64668587778284,-1.25210197041621,-1.50285884310738));
#7471=CARTESIAN_POINT('Ctrl Pts',(6.60041327654971,-1.3088984223833,-1.50746139371859));
#7472=CARTESIAN_POINT('Ctrl Pts',(6.55821191719384,-1.35594830603633,-1.51127886768112));
#7473=CARTESIAN_POINT('Ctrl Pts',(6.42201158970083,-1.49400525578319,-1.52278028367437));
#7474=CARTESIAN_POINT('Ctrl Pts',(6.32124652972505,-1.5778371325406,-1.53022112715308));
#7475=CARTESIAN_POINT('Ctrl Pts',(6.13925881703669,-1.70118655634368,-1.54315386280845));
#7476=CARTESIAN_POINT('Ctrl Pts',(6.06226281206282,-1.74616509531594,-1.54849118000131));
#7477=CARTESIAN_POINT('Ctrl Pts',(5.96850269381051,-1.79282335723927,-1.55499066383679));
#7478=CARTESIAN_POINT('Ctrl Pts',(5.95439878359246,-1.79963589060291,-1.55596815772121));
#7479=CARTESIAN_POINT('Ctrl Pts',(5.93111553709109,-1.81054597854394,-1.55758225395842));
#7480=CARTESIAN_POINT('Ctrl Pts',(5.92198269523603,-1.81474157125658,-1.55821548405231));
#7481=CARTESIAN_POINT('Ctrl Pts',(5.90548925022832,-1.82216816416182,-1.55935942812834));
#7482=CARTESIAN_POINT('Ctrl Pts',(5.89814003881371,-1.8254240485874,-1.5598692793393));
#7483=CARTESIAN_POINT('Ctrl Pts',(5.88241021177907,-1.83227932207668,-1.56096090478734));
#7484=CARTESIAN_POINT('Ctrl Pts',(5.87402421041016,-1.83586581800781,-1.56154310259313));
#7485=CARTESIAN_POINT('Ctrl Pts',(5.85123284343791,-1.8454287891068,-1.56312614820089));
#7486=CARTESIAN_POINT('Ctrl Pts',(5.8367817441206,-1.85129393889771,-1.56413071206119));
#7487=CARTESIAN_POINT('Ctrl Pts',(5.75945520057769,-1.88162663463422,-1.56951156482025));
#7488=CARTESIAN_POINT('Ctrl Pts',(5.69544406989846,-1.90305933057875,-1.57398736994295));
#7489=CARTESIAN_POINT('Ctrl Pts',(5.47327113697508,-1.9651186959548,-1.58959726260307));
#7490=CARTESIAN_POINT('Ctrl Pts',(5.31127463664889,-1.98956670050335,-1.60116491633589));
#7491=CARTESIAN_POINT('Ctrl Pts',(5.09289479782387,-1.99551531734772,-1.61615596848631));
#7492=CARTESIAN_POINT('Ctrl Pts',(5.03760171519455,-1.99472357592404,-1.6198930803525));
#7493=CARTESIAN_POINT('Ctrl Pts',(4.97313366120662,-1.99111700440142,-1.6241310108593));
#7494=CARTESIAN_POINT('Ctrl Pts',(4.96386286024713,-1.99053337944126,-1.62473754077677));
#7495=CARTESIAN_POINT('Ctrl Pts',(4.94884631802394,-1.98948268226163,-1.62571490848222));
#7496=CARTESIAN_POINT('Ctrl Pts',(4.94309805552074,-1.98905543579943,-1.62608783512299));
#7497=CARTESIAN_POINT('Ctrl Pts',(4.93286046947233,-1.98824987966763,-1.62674976891576));
#7498=CARTESIAN_POINT('Ctrl Pts',(4.92837050167491,-1.9878812728814,-1.62703930253347));
#7499=CARTESIAN_POINT('Ctrl Pts',(4.91862150306144,-1.98704766264577,-1.62766626559148));
#7500=CARTESIAN_POINT('Ctrl Pts',(4.91336306038342,-1.98657699226482,-1.62800337757333));
#7501=CARTESIAN_POINT('Ctrl Pts',(4.89853393341771,-1.98519030693725,-1.62895121534531));
#7502=CARTESIAN_POINT('Ctrl Pts',(4.88896776112337,-1.98422595352618,-1.62955932141436));
#7503=CARTESIAN_POINT('Ctrl Pts',(4.82843158041389,-1.97768091359596,-1.63338847261488));
#7504=CARTESIAN_POINT('Ctrl Pts',(4.77768100065934,-1.97020537075589,-1.63651324264127));
#7505=CARTESIAN_POINT('Ctrl Pts',(4.5763949731471,-1.93257611911304,-1.64876347564443));
#7506=CARTESIAN_POINT('Ctrl Pts',(4.42927300728366,-1.88705067219852,-1.65743153142407));
#7507=CARTESIAN_POINT('Ctrl Pts',(4.2157942573648,-1.79289041213985,-1.67121740888998));
#7508=CARTESIAN_POINT('Ctrl Pts',(4.14477520687709,-1.75633026346884,-1.67602103355296));
#7509=CARTESIAN_POINT('Ctrl Pts',(4.06298206147126,-1.70781148698273,-1.68192603608728));
#7510=CARTESIAN_POINT('Ctrl Pts',(4.04991273995426,-1.69985421600065,-1.68288131228921));
#7511=CARTESIAN_POINT('Ctrl Pts',(4.02850636709828,-1.68648094716839,-1.68446615631666));
#7512=CARTESIAN_POINT('Ctrl Pts',(4.02011581218113,-1.68115148420791,-1.68509256068817));
#7513=CARTESIAN_POINT('Ctrl Pts',(4.00502023517102,-1.6714040573979,-1.68622915443043));
#7514=CARTESIAN_POINT('Ctrl Pts',(3.99830135145635,-1.66700787114163,-1.68673852935459));
#7515=CARTESIAN_POINT('Ctrl Pts',(3.98394342631604,-1.65748914436901,-1.68783464915381));
#7516=CARTESIAN_POINT('Ctrl Pts',(3.97631292981377,-1.65235411057693,-1.68842185372859));
#7517=CARTESIAN_POINT('Ctrl Pts',(3.95554972286836,-1.6381716544067,-1.69003268024754));
#7518=CARTESIAN_POINT('Ctrl Pts',(3.94248979186402,-1.62901937791495,-1.69106024315119));
#7519=CARTESIAN_POINT('Ctrl Pts',(3.87016143092115,-1.57702809668791,-1.69683328265526));
#7520=CARTESIAN_POINT('Ctrl Pts',(3.81318067113999,-1.53111651544855,-1.70169652706301));
#7521=CARTESIAN_POINT('Ctrl Pts',(3.61255882237539,-1.35042064660988,-1.720028856873));
#7522=CARTESIAN_POINT('Ctrl Pts',(3.48659610216878,-1.19774315429533,-1.73415325122234));
#7523=CARTESIAN_POINT('Ctrl Pts',(3.374306119416,-1.01129003143331,-1.74866593791251));
#7524=CARTESIAN_POINT('Ctrl Pts',(3.36385503599482,-0.993305929066541,-1.75003925240561));
#7525=CARTESIAN_POINT('Ctrl Pts',(3.35006116952603,-0.968691255488288,-1.75187995194017));
#7526=CARTESIAN_POINT('Ctrl Pts',(3.34647170970935,-0.962201388766289,-1.75236164985777));
#7527=CARTESIAN_POINT('Ctrl Pts',(3.34084932748408,-0.951900703247766,-1.75312030978925));
#7528=CARTESIAN_POINT('Ctrl Pts',(3.33879248700933,-0.94810312077189,-1.75339874893728));
#7529=CARTESIAN_POINT('Ctrl Pts',(3.33457180739576,-0.940249602439723,-1.75397192985947));
#7530=CARTESIAN_POINT('Ctrl Pts',(3.33240964403256,-0.936192846267882,-1.75426655451327));
#7531=CARTESIAN_POINT('Ctrl Pts',(3.32725188957452,-0.926434494890934,-1.7549718548187));
#7532=CARTESIAN_POINT('Ctrl Pts',(3.32426981851092,-0.920725734059634,-1.75538168749883));
#7533=CARTESIAN_POINT('Ctrl Pts',(3.31408414040363,-0.900994385267099,-1.75678899992654));
#7534=CARTESIAN_POINT('Ctrl Pts',(3.30701892827018,-0.886900489123544,-1.75777827632187));
#7535=CARTESIAN_POINT('Ctrl Pts',(3.26550157265754,-0.80157002832534,-1.76368119422108));
#7536=CARTESIAN_POINT('Ctrl Pts',(3.23514233688776,-0.728410939277028,-1.7683832248744));
#7537=CARTESIAN_POINT('Ctrl Pts',(3.19116541366846,-0.601612518618675,-1.77624342920264));
#7538=CARTESIAN_POINT('Ctrl Pts',(3.17528441653814,-0.548865452274119,-1.77943226326048));
#7539=CARTESIAN_POINT('Ctrl Pts',(3.12985329458514,-0.371715135196965,-1.7900517899023));
#7540=CARTESIAN_POINT('Ctrl Pts',(3.11007804444024,-0.245152309848009,-1.79751608522849));
#7541=CARTESIAN_POINT('Ctrl Pts',(3.10108422514295,-0.0928309925308564,
-1.80690246507649));
#7542=CARTESIAN_POINT('Ctrl Pts',(3.10008459530949,-0.0680624661680096,
-1.80844039725096));
#7543=CARTESIAN_POINT('Ctrl Pts',(3.09932720458535,-0.0331650522634131,
-1.81062633069008));
#7544=CARTESIAN_POINT('Ctrl Pts',(3.09918462038584,-0.0230461708683548,
-1.8112624170591));
#7545=CARTESIAN_POINT('Ctrl Pts',(3.09907030950185,-0.00540707666466319,
-1.81237534388369));
#7546=CARTESIAN_POINT('Ctrl Pts',(3.09906410068734,0.00211276621998525,
-1.81285110494454));
#7547=CARTESIAN_POINT('Ctrl Pts',(3.09914016723497,0.0178650461105865,-1.81385051894081));
#7548=CARTESIAN_POINT('Ctrl Pts',(3.09923088819271,0.0260972823136664,-1.81437442548822));
#7549=CARTESIAN_POINT('Ctrl Pts',(3.09956878121841,0.045728490073413,-1.8156277120367));
#7550=CARTESIAN_POINT('Ctrl Pts',(3.09986272779776,0.0571262667256657,-1.81635853335772));
#7551=CARTESIAN_POINT('Ctrl Pts',(3.10119839893522,0.0959868948211802,-1.8188614166134));
#7552=CARTESIAN_POINT('Ctrl Pts',(3.10270990775319,0.123429440423981,-1.82064796080307));
#7553=CARTESIAN_POINT('Ctrl Pts',(3.10771576720183,0.189442774388229,-1.82499354244146));
#7554=CARTESIAN_POINT('Ctrl Pts',(3.11176726212538,0.227958904195587,-1.82756878706819));
#7555=CARTESIAN_POINT('Ctrl Pts',(3.13215891140683,0.379319795090397,-1.83784551027739));
#7556=CARTESIAN_POINT('Ctrl Pts',(3.15703834481352,0.490784732535586,-1.84577482906485));
#7557=CARTESIAN_POINT('Ctrl Pts',(3.22285594812107,0.699658234463698,-1.86104201299441));
#7558=CARTESIAN_POINT('Ctrl Pts',(3.26227883319992,0.797176251632727,-1.8683496531302));
#7559=CARTESIAN_POINT('Ctrl Pts',(3.31647981299466,0.905720394206073,-1.87639215639055));
#7560=CARTESIAN_POINT('Ctrl Pts',(3.32393699594441,0.920207515825462,-1.87746338280441));
#7561=CARTESIAN_POINT('Ctrl Pts',(3.33471702848311,0.940534000899643,-1.87896160187262));
#7562=CARTESIAN_POINT('Ctrl Pts',(3.33789291743876,0.94644999897255,-1.87939707654038));
#7563=CARTESIAN_POINT('Ctrl Pts',(3.34329574346284,0.956393494073345,-1.88012789017254));
#7564=CARTESIAN_POINT('Ctrl Pts',(3.34550683753067,0.960429491069186,-1.88042420799356));
#7565=CARTESIAN_POINT('Ctrl Pts',(3.35006398123735,0.968679936332645,-1.88102924594712));
#7566=CARTESIAN_POINT('Ctrl Pts',(3.35241137756574,0.972893579240374,-1.88133787818584));
#7567=CARTESIAN_POINT('Ctrl Pts',(3.3584687166546,0.983674510629271,-1.88212669297813));
#7568=CARTESIAN_POINT('Ctrl Pts',(3.36220070656579,0.990229417773981,-1.882605492478));
#7569=CARTESIAN_POINT('Ctrl Pts',(3.37784597404471,1.01734999331573,-1.88458380860641));
#7570=CARTESIAN_POINT('Ctrl Pts',(3.3900896917811,1.03772404623634,-1.88606354420312));
#7571=CARTESIAN_POINT('Ctrl Pts',(3.42384956451334,1.09169296900248,-1.88997924537867));
#7572=CARTESIAN_POINT('Ctrl Pts',(3.44601483621355,1.12487050229805,-1.89238227155398));
#7573=CARTESIAN_POINT('Ctrl Pts',(3.52308446842537,1.23305816293596,-1.90028144822588));
#7574=CARTESIAN_POINT('Ctrl Pts',(3.58223414171343,1.30489587443794,-1.90563612008514));
#7575=CARTESIAN_POINT('Ctrl Pts',(3.73568729464565,1.46676859989317,-1.91860062568755));
#7576=CARTESIAN_POINT('Ctrl Pts',(3.83420393443117,1.55219101579464,-1.92624130773067));
#7577=CARTESIAN_POINT('Ctrl Pts',(3.95354995120486,1.63678286629157,-1.93531306357665));
#7578=CARTESIAN_POINT('Ctrl Pts',(3.96688642258813,1.64599356452771,-1.93632399352648));
#7579=CARTESIAN_POINT('Ctrl Pts',(3.98880905762478,1.66074288210554,-1.93798204858651));
#7580=CARTESIAN_POINT('Ctrl Pts',(3.99732831022964,1.66637996663326,-1.93862547613114));
#7581=CARTESIAN_POINT('Ctrl Pts',(4.01264115702831,1.67634401859768,-1.93978058429788));
#7582=CARTESIAN_POINT('Ctrl Pts',(4.01941841414815,1.6806957741929,-1.94029132997025));
#7583=CARTESIAN_POINT('Ctrl Pts',(4.0338385931314,1.68983227459826,-1.94137712264019));
#7584=CARTESIAN_POINT('Ctrl Pts',(4.04148795619025,1.69460646577168,-1.94195254322311));
#7585=CARTESIAN_POINT('Ctrl Pts',(4.06205175543019,1.70724800805633,-1.94349812617435));
#7586=CARTESIAN_POINT('Ctrl Pts',(4.07502352197986,1.71502051670292,-1.94447171027733));
#7587=CARTESIAN_POINT('Ctrl Pts',(4.14054028501352,1.7532716793363,-1.94938317749088));
#7588=CARTESIAN_POINT('Ctrl Pts',(4.1943648702007,1.78148357840924,-1.95340094019957));
#7589=CARTESIAN_POINT('Ctrl Pts',(4.36560427091852,1.86149781037265,-1.96613695666556));
#7590=CARTESIAN_POINT('Ctrl Pts',(4.48677739467328,1.90445962130019,-1.97510646505271));
#7591=CARTESIAN_POINT('Ctrl Pts',(4.70481567651747,1.95882689511632,-1.99074759218179));
#7592=CARTESIAN_POINT('Ctrl Pts',(4.79999444564586,1.97534793080907,-1.99740927664585));
#7593=CARTESIAN_POINT('Ctrl Pts',(4.90690167216118,1.98600260511815,-2.0044707704093));
#7594=CARTESIAN_POINT('Ctrl Pts',(4.91780760347756,1.98699889635208,-2.00518623091826));
#7595=CARTESIAN_POINT('Ctrl Pts',(4.93433451862203,1.98837154095326,-2.00626246984286));
#7596=CARTESIAN_POINT('Ctrl Pts',(4.93994959347915,1.98881396411933,-2.00662673362541));
#7597=CARTESIAN_POINT('Ctrl Pts',(4.95005103741942,1.9895668404777,-2.00727944599431));
#7598=CARTESIAN_POINT('Ctrl Pts',(4.9545366285985,1.98988591008562,-2.00756836045675));
#7599=CARTESIAN_POINT('Ctrl Pts',(4.96439377948814,1.99055357549616,-2.00820121920363));
#7600=CARTESIAN_POINT('Ctrl Pts',(4.96976567951689,1.99089559936241,-2.00854479650785));
#7601=CARTESIAN_POINT('Ctrl Pts',(4.98521925860994,1.99181672359592,-2.00952956851799));
#7602=CARTESIAN_POINT('Ctrl Pts',(4.99530421028151,1.99234102879653,-2.01016780868806));
#7603=CARTESIAN_POINT('Ctrl Pts',(5.06847692451208,1.99558822214792,-2.01476942041657));
#7604=CARTESIAN_POINT('Ctrl Pts',(5.13166528471118,1.99539093417366,-2.01858605471588));
#7605=CARTESIAN_POINT('Ctrl Pts',(5.32719508098362,1.98548615311052,-2.03019711301372));
#7606=CARTESIAN_POINT('Ctrl Pts',(5.45864981989365,1.96558466732515,-2.03773976363913));
#7607=CARTESIAN_POINT('Ctrl Pts',(5.67173539166069,1.91119555815945,-2.05068642434002));
#7608=CARTESIAN_POINT('Ctrl Pts',(5.75479205074167,1.88408307746055,-2.05592046699359));
#7609=CARTESIAN_POINT('Ctrl Pts',(5.85031598601377,1.84580517650454,-2.06230721219072));
#7610=CARTESIAN_POINT('Ctrl Pts',(5.8647624153107,1.8398181714033,-2.06328316210525));
#7611=CARTESIAN_POINT('Ctrl Pts',(5.88836844798812,1.82970832515533,-2.06489522657505));
#7612=CARTESIAN_POINT('Ctrl Pts',(5.89757011977773,1.82568498434705,-2.06552798357116));
#7613=CARTESIAN_POINT('Ctrl Pts',(5.91408067683418,1.81831689333237,-2.06667141482714));
#7614=CARTESIAN_POINT('Ctrl Pts',(5.92140051558812,1.81499710590205,-2.06718122966382));
#7615=CARTESIAN_POINT('Ctrl Pts',(5.92884851008935,1.81156477293497,-2.06770296546701));
#7616=CARTESIAN_POINT('Ctrl Pts',(5.92899700691455,1.81149631753623,-2.06771336896331));
#7617=CARTESIAN_POINT('Ctrl Pts',(5.9292823162582,1.81136475053615,-2.06773335970989));
#7618=CARTESIAN_POINT('Ctrl Pts',(5.92941913005179,1.81130164168948,-2.06774294686551));
#7619=CARTESIAN_POINT('Ctrl Pts',(5.92968201915897,1.81118034126934,-2.06776137067221));
#7620=CARTESIAN_POINT('Ctrl Pts',(5.92980809555902,1.81112215202644,-2.06777020724352));
#7621=CARTESIAN_POINT('Ctrl Pts',(5.93005037719339,1.81101029878513,-2.06778719021585));
#7622=CARTESIAN_POINT('Ctrl Pts',(5.93016658334015,1.81095663676551,-2.06779533654865));
#7623=CARTESIAN_POINT('Ctrl Pts',(5.93038991960546,1.81085347780007,-2.0678109943993));
#7624=CARTESIAN_POINT('Ctrl Pts',(5.93049705050445,1.81080398252864,-2.06781850585978));
#7625=CARTESIAN_POINT('Ctrl Pts',(5.93070296526726,1.81070882620346,-2.06783294475181));
#7626=CARTESIAN_POINT('Ctrl Pts',(5.93080174978758,1.81066316657235,-2.0678398721343));
#7627=CARTESIAN_POINT('Ctrl Pts',(5.93099164016013,1.81057537764115,-2.0678531894628));
#7628=CARTESIAN_POINT('Ctrl Pts',(5.9310827465768,1.8105332495448,-2.06785957936768));
#7629=CARTESIAN_POINT('Ctrl Pts',(5.93125789365983,1.81045224454577,-2.06787186449336));
#7630=CARTESIAN_POINT('Ctrl Pts',(5.9313419348035,1.81041336866582,-2.06787775967909));
#7631=CARTESIAN_POINT('Ctrl Pts',(5.93150351354332,1.81033861166806,-2.06788909460288));
#7632=CARTESIAN_POINT('Ctrl Pts',(5.93158105153806,1.81030273142202,-2.06789453431068));
#7633=CARTESIAN_POINT('Ctrl Pts',(5.93173013976533,1.81023373010148,-2.06790499429368));
#7634=CARTESIAN_POINT('Ctrl Pts',(5.93180169034993,1.8102006097615,-2.06791001454411));
#7635=CARTESIAN_POINT('Ctrl Pts',(5.93193927715159,1.81013691174393,-2.06791966868298));
#7636=CARTESIAN_POINT('Ctrl Pts',(5.93200531366934,1.81010633469004,-2.06792430255046));
#7637=CARTESIAN_POINT('Ctrl Pts',(5.93213230695122,1.81004752423371,-2.06793321429796));
#7638=CARTESIAN_POINT('Ctrl Pts',(5.93219326396951,1.81001929136236,-2.06793749216006));
#7639=CARTESIAN_POINT('Ctrl Pts',(5.93231049747237,1.80996498626438,-2.06794571980887));
#7640=CARTESIAN_POINT('Ctrl Pts',(5.93236677414189,1.80993891450404,-2.06794966957813));
#7641=CARTESIAN_POINT('Ctrl Pts',(5.93250958038024,1.80987274738125,-2.06795969285791));
#7642=CARTESIAN_POINT('Ctrl Pts',(5.93259610830154,1.8098326484326,-2.0679657664927));
#7643=CARTESIAN_POINT('Ctrl Pts',(5.93276767924201,1.80975312372476,-2.06797781035748));
#7644=CARTESIAN_POINT('Ctrl Pts',(5.93285272235516,1.80971369817753,-2.06798378057997));
#7645=CARTESIAN_POINT('Ctrl Pts',(5.93302135799563,1.80963550512518,-2.06799561998734));
#7646=CARTESIAN_POINT('Ctrl Pts',(5.93310495061014,1.80959673782502,-2.0680014891648));
#7647=CARTESIAN_POINT('Ctrl Pts',(5.94188927979675,1.8055221368139,-2.06861829244457));
#7648=CARTESIAN_POINT('Ctrl Pts',(5.9505606704281,1.80142366818618,-2.06923137467807));
#7649=CARTESIAN_POINT('Ctrl Pts',(5.97545962206154,1.78943492256857,-2.0710041264902));
#7650=CARTESIAN_POINT('Ctrl Pts',(5.99160977767954,1.78138695295338,-2.0721692189174));
#7651=CARTESIAN_POINT('Ctrl Pts',(6.02793282923505,1.76266698883203,-2.07482506153702));
#7652=CARTESIAN_POINT('Ctrl Pts',(6.04803594204269,1.75186581803919,-2.07632017285381));
#7653=CARTESIAN_POINT('Ctrl Pts',(6.11276257030876,1.71564430585971,-2.08121778490656));
#7654=CARTESIAN_POINT('Ctrl Pts',(6.15658793285239,1.68884681548474,-2.08466625592449));
#7655=CARTESIAN_POINT('Ctrl Pts',(6.297264134024,1.59518351362657,-2.09617054623165));
#7656=CARTESIAN_POINT('Ctrl Pts',(6.38923361596424,1.52144310940326,-2.10441913208435));
#7657=CARTESIAN_POINT('Ctrl Pts',(6.53780282432056,1.37903358794513,-2.11872097298468));
#7658=CARTESIAN_POINT('Ctrl Pts',(6.59733894861155,1.31387034900419,-2.12478531565143));
#7659=CARTESIAN_POINT('Ctrl Pts',(6.65920296503921,1.23642463521693,-2.13130014555501));
#7660=CARTESIAN_POINT('Ctrl Pts',(6.66596226204759,1.22781860359573,-2.13201506090664));
#7661=CARTESIAN_POINT('Ctrl Pts',(6.67609190665993,1.21470058999055,-2.13309064489747));
#7662=CARTESIAN_POINT('Ctrl Pts',(6.67951440385955,1.21022940732468,-2.13345479273994));
#7663=CARTESIAN_POINT('Ctrl Pts',(6.68563613265604,1.20216137196907,-2.13410738372912));
#7664=CARTESIAN_POINT('Ctrl Pts',(6.68834216205974,1.19856984737877,-2.13439629193668));
#7665=CARTESIAN_POINT('Ctrl Pts',(6.69426153818052,1.19065794349972,-2.13502923874101));
#7666=CARTESIAN_POINT('Ctrl Pts',(6.69746954355457,1.18633369865247,-2.13537290965031));
#7667=CARTESIAN_POINT('Ctrl Pts',(6.70664794654209,1.17385636869069,-2.13635822037577));
#7668=CARTESIAN_POINT('Ctrl Pts',(6.7125740533571,1.16567069497755,-2.13699690063305));
#7669=CARTESIAN_POINT('Ctrl Pts',(6.7551975335594,1.10584335771317,-2.14161184268976));
#7670=CARTESIAN_POINT('Ctrl Pts',(6.78948242457366,1.05251888617775,-2.14544039818007));
#7671=CARTESIAN_POINT('Ctrl Pts',(6.88917915974975,0.879901948210566,-2.1572608929734));
#7672=CARTESIAN_POINT('Ctrl Pts',(6.94496855236489,0.755509551438774,-2.16498676156849));
#7673=CARTESIAN_POINT('Ctrl Pts',(7.00455075623325,0.575371358662103,-2.17617400497363));
#7674=CARTESIAN_POINT('Ctrl Pts',(7.01935974533257,0.523679781749934,-2.17938068596302));
#7675=CARTESIAN_POINT('Ctrl Pts',(7.04095495856879,0.434898167312737,-2.1849344434968));
#7676=CARTESIAN_POINT('Ctrl Pts',(7.04881068916503,0.398098228737879,-2.18724945218381));
#7677=CARTESIAN_POINT('Ctrl Pts',(7.05802773711904,0.348023591918383,-2.1904271058849));
#7678=CARTESIAN_POINT('Ctrl Pts',(7.06030379602823,0.334923803400872,-2.19126090328228));
#7679=CARTESIAN_POINT('Ctrl Pts',(7.0638389147781,0.313297771354655,-2.19264193188578));
#7680=CARTESIAN_POINT('Ctrl Pts',(7.06517400074274,0.304784246989489,-2.19318675581137));
#7681=CARTESIAN_POINT('Ctrl Pts',(7.06759305274723,0.288677289587745,-2.19421981341622));
#7682=CARTESIAN_POINT('Ctrl Pts',(7.06868847042942,0.281085714271129,-2.19470767627308));
#7683=CARTESIAN_POINT('Ctrl Pts',(7.0708314196408,0.265603208538821,-2.195704668048));
#7684=CARTESIAN_POINT('Ctrl Pts',(7.07187555478401,0.257711955254293,-2.19621389442358));
#7685=CARTESIAN_POINT('Ctrl Pts',(7.07418209936535,0.239439391289865,-2.1973955915975));
#7686=CARTESIAN_POINT('Ctrl Pts',(7.07541014876699,0.229054054103397,-2.19806912603359));
#7687=CARTESIAN_POINT('Ctrl Pts',(7.07947027967402,0.192238214384171,-2.20046378649389));
#7688=CARTESIAN_POINT('Ctrl Pts',(7.0818555550484,0.16576223376657,-2.20219869070669));
#7689=CARTESIAN_POINT('Ctrl Pts',(7.08698906676703,0.0924029900823677,-2.20704281944523));
#7690=CARTESIAN_POINT('Ctrl Pts',(7.08861168295073,0.0454612257313511,-2.21018466912641));
#7691=CARTESIAN_POINT('Ctrl Pts',(7.0885765985467,-0.00149056292464214,
-2.21336761392587));
#7692=CARTESIAN_POINT('Ctrl Pts',(7.0885770951979,-0.000490293958327712,
-2.37086699796518));
#7693=CARTESIAN_POINT('Ctrl Pts',(7.08858062860284,0.0138852845779169,-2.36996691156082));
#7694=CARTESIAN_POINT('Ctrl Pts',(7.08842876113032,0.0282610016564163,-2.36907436554716));
#7695=CARTESIAN_POINT('Ctrl Pts',(7.08465333163941,0.204863214486289,-2.35818874130353));
#7696=CARTESIAN_POINT('Ctrl Pts',(7.06140305434961,0.366083502392327,-2.34903163477475));
#7697=CARTESIAN_POINT('Ctrl Pts',(6.9941308187758,0.613829127704159,-2.33401184281283));
#7698=CARTESIAN_POINT('Ctrl Pts',(6.9629579969907,0.703055498021072,-2.3284018228086));
#7699=CARTESIAN_POINT('Ctrl Pts',(6.91643565497422,0.810962553252018,-2.32115677411448));
#7700=CARTESIAN_POINT('Ctrl Pts',(6.90691504659619,0.832030189079554,-2.31971987530524));
#7701=CARTESIAN_POINT('Ctrl Pts',(6.89247926954782,0.862549385337824,-2.31760318736121));
#7702=CARTESIAN_POINT('Ctrl Pts',(6.88785091826512,0.872135081926787,-2.31693322188843));
#7703=CARTESIAN_POINT('Ctrl Pts',(6.87956229407106,0.888956309554531,-2.31574824533235));
#7704=CARTESIAN_POINT('Ctrl Pts',(6.87593418125697,0.896207482125178,-2.31523435814891));
#7705=CARTESIAN_POINT('Ctrl Pts',(6.86827843090544,0.911278001215554,-2.3141597874125));
#7706=CARTESIAN_POINT('Ctrl Pts',(6.86424308955388,0.919093216528032,-2.31359884286087));
#7707=CARTESIAN_POINT('Ctrl Pts',(6.85359831041912,0.939378641736502,-2.31213303788419));
#7708=CARTESIAN_POINT('Ctrl Pts',(6.84690807096786,0.951805671942332,-2.31122534924936));
#7709=CARTESIAN_POINT('Ctrl Pts',(6.8187733172895,1.00276252617067,-2.30746234454801));
#7710=CARTESIAN_POINT('Ctrl Pts',(6.79618737235399,1.04064457502452,-2.30456678225045));
#7711=CARTESIAN_POINT('Ctrl Pts',(6.68013903614349,1.22138463343181,-2.29025558967698));
#7712=CARTESIAN_POINT('Ctrl Pts',(6.5698633972145,1.35257722953066,-2.27822523191417));
#7713=CARTESIAN_POINT('Ctrl Pts',(6.40722685475483,1.50217907212634,-2.26293643992146));
#7714=CARTESIAN_POINT('Ctrl Pts',(6.36890536313873,1.53484102589633,-2.25948574374275));
#7715=CARTESIAN_POINT('Ctrl Pts',(6.31474041008112,1.57757613034927,-2.25485170157798));
#7716=CARTESIAN_POINT('Ctrl Pts',(6.29993186502775,1.58892640042156,-2.2536084669937));
#7717=CARTESIAN_POINT('Ctrl Pts',(6.27742159942448,1.60568371985401,-2.25175652205332));
#7718=CARTESIAN_POINT('Ctrl Pts',(6.26983770636503,1.61124647650269,-2.25113891960059));
#7719=CARTESIAN_POINT('Ctrl Pts',(6.25746046607455,1.62019118824391,-2.25014156837339));
#7720=CARTESIAN_POINT('Ctrl Pts',(6.25269114439442,1.62360593286225,-2.24975978584511));
#7721=CARTESIAN_POINT('Ctrl Pts',(6.24352136900703,1.63011032935057,-2.24903068456829));
#7722=CARTESIAN_POINT('Ctrl Pts',(6.23912335728919,1.63320331931891,-2.2486831496498));
#7723=CARTESIAN_POINT('Ctrl Pts',(6.23469423101349,1.63629150181637,-2.24833536008383));
#7724=CARTESIAN_POINT('Ctrl Pts',(6.23467563032359,1.63630447056771,-2.24833389953539));
#7725=CARTESIAN_POINT('Ctrl Pts',(6.23463797992693,1.63633072017934,-2.24833094325997));
#7726=CARTESIAN_POINT('Ctrl Pts',(6.23461893009051,1.63634400110702,-2.24832944752471));
#7727=CARTESIAN_POINT('Ctrl Pts',(6.23458036492786,1.63637088648601,-2.24832641958799));
#7728=CARTESIAN_POINT('Ctrl Pts',(6.2345608496664,1.63638449086773,-2.24832488739365));
#7729=CARTESIAN_POINT('Ctrl Pts',(6.23452133644111,1.63641203507991,-2.24832178519349));
#7730=CARTESIAN_POINT('Ctrl Pts',(6.23450133839714,1.63642597494027,-2.24832021518353));
#7731=CARTESIAN_POINT('Ctrl Pts',(6.23446084144457,1.63645420269126,-2.24831703593276));
#7732=CARTESIAN_POINT('Ctrl Pts',(6.23444034257257,1.63646849052878,-2.24831542669711));
#7733=CARTESIAN_POINT('Ctrl Pts',(6.23083342070655,1.63898243614546,-2.24803227859395));
#7734=CARTESIAN_POINT('Ctrl Pts',(6.2272388254637,1.64147027397583,-2.24775155250582));
#7735=CARTESIAN_POINT('Ctrl Pts',(6.21908958129172,1.64707087514468,-2.24711839296449));
#7736=CARTESIAN_POINT('Ctrl Pts',(6.21453018859606,1.6501765687392,-2.2467664348131));
#7737=CARTESIAN_POINT('Ctrl Pts',(6.20150531677765,1.65896975944463,-2.24576730595274));
#7738=CARTESIAN_POINT('Ctrl Pts',(6.1930088798427,1.66461140178497,-2.24512310395784));
#7739=CARTESIAN_POINT('Ctrl Pts',(6.13628659719297,1.70165137727086,-2.24086967605587));
#7740=CARTESIAN_POINT('Ctrl Pts',(6.08675989570854,1.73101848673347,-2.23738097778244));
#7741=CARTESIAN_POINT('Ctrl Pts',(5.89402619583833,1.83430211435706,-2.2243701029479));
#7742=CARTESIAN_POINT('Ctrl Pts',(5.74332723460475,1.892917669139,-2.21528738380476));
#7743=CARTESIAN_POINT('Ctrl Pts',(5.52215376724536,1.94937741091136,-2.2016958874161));
#7744=CARTESIAN_POINT('Ctrl Pts',(5.45630435265326,1.96268816747233,-2.19762598486409));
#7745=CARTESIAN_POINT('Ctrl Pts',(5.37451182492044,1.97496487196394,-2.1924809207216));
#7746=CARTESIAN_POINT('Ctrl Pts',(5.35908360926192,1.97709613355135,-2.19150664607561));
#7747=CARTESIAN_POINT('Ctrl Pts',(5.334588001054,1.98018809241791,-2.18995312469982));
#7748=CARTESIAN_POINT('Ctrl Pts',(5.32553605181541,1.98126768737313,-2.18937761257643));
#7749=CARTESIAN_POINT('Ctrl Pts',(5.30848859560037,1.98318245518445,-2.18829092403521));
#7750=CARTESIAN_POINT('Ctrl Pts',(5.30049479754256,1.9840314178617,-2.18778019100062));
#7751=CARTESIAN_POINT('Ctrl Pts',(5.28248873054808,1.98583371031093,-2.18662703448826));
#7752=CARTESIAN_POINT('Ctrl Pts',(5.27247400231071,1.98675967669244,-2.18598376837826));
#7753=CARTESIAN_POINT('Ctrl Pts',(5.24682315798228,1.98893585397185,-2.18433112647639));
#7754=CARTESIAN_POINT('Ctrl Pts',(5.23117875265129,1.99007741646309,-2.18331839556056));
#7755=CARTESIAN_POINT('Ctrl Pts',(5.12594088808117,1.9965097502446,-2.17647232762051));
#7756=CARTESIAN_POINT('Ctrl Pts',(5.03610420952479,1.99593250143225,-2.17045775765614));
#7757=CARTESIAN_POINT('Ctrl Pts',(4.81681462188701,1.97970548733625,-2.15538958529781));
#7758=CARTESIAN_POINT('Ctrl Pts',(4.68826878170434,1.95741898932754,-2.14620967108578));
#7759=CARTESIAN_POINT('Ctrl Pts',(4.50202491027066,1.90598397309354,-2.1329026529644));
#7760=CARTESIAN_POINT('Ctrl Pts',(4.44205874730041,1.88632034143467,-2.12862243982622));
#7761=CARTESIAN_POINT('Ctrl Pts',(4.37368662223361,1.8602492015479,-2.12382159946081));
#7762=CARTESIAN_POINT('Ctrl Pts',(4.36428093490859,1.85658067472828,-2.12316297327043));
#7763=CARTESIAN_POINT('Ctrl Pts',(4.34990406940519,1.85084709564284,-2.12215946213798));
#7764=CARTESIAN_POINT('Ctrl Pts',(4.34491288554786,1.84883313129778,-2.1218116738586));
#7765=CARTESIAN_POINT('Ctrl Pts',(4.3357663996273,1.84509936747695,-2.12117552298269));
#7766=CARTESIAN_POINT('Ctrl Pts',(4.33160876815354,1.84338572096059,-2.12088681207999));
#7767=CARTESIAN_POINT('Ctrl Pts',(4.32225609175746,1.83949378568759,-2.12023836325715));
#7768=CARTESIAN_POINT('Ctrl Pts',(4.31706446492211,1.83730754594363,-2.11987910814428));
#7769=CARTESIAN_POINT('Ctrl Pts',(4.30180470084323,1.83080528358261,-2.11882500286456));
#7770=CARTESIAN_POINT('Ctrl Pts',(4.29176258266189,1.82642820521991,-2.11813370462089));
#7771=CARTESIAN_POINT('Ctrl Pts',(4.19929161178927,1.78521292794018,-2.11178556685109));
#7772=CARTESIAN_POINT('Ctrl Pts',(4.11940562575843,1.74289586546341,-2.10642867273829));
#7773=CARTESIAN_POINT('Ctrl Pts',(3.94510813087981,1.63482274301659,-2.09443648937829));
#7774=CARTESIAN_POINT('Ctrl Pts',(3.85296696157566,1.56603533502187,-2.08786212961973));
#7775=CARTESIAN_POINT('Ctrl Pts',(3.72856822254267,1.45525897450899,-2.07800688076357));
#7776=CARTESIAN_POINT('Ctrl Pts',(3.69124327960925,1.41931974226747,-2.07490444260612));
#7777=CARTESIAN_POINT('Ctrl Pts',(3.63171180254486,1.35735459229981,-2.06966244340371));
#7778=CARTESIAN_POINT('Ctrl Pts',(3.60869953293345,1.33213682710641,-2.06755628576632));
#7779=CARTESIAN_POINT('Ctrl Pts',(3.5782266737681,1.29697204080412,-2.06464814789894));
#7780=CARTESIAN_POINT('Ctrl Pts',(3.57019445927486,1.28752657868965,-2.06386974606849));
#7781=CARTESIAN_POINT('Ctrl Pts',(3.55685139506303,1.27153611915698,-2.06255619943343));
#7782=CARTESIAN_POINT('Ctrl Pts',(3.55149295796404,1.26503114984298,-2.06202299949656));
#7783=CARTESIAN_POINT('Ctrl Pts',(3.54099900883453,1.25212604883943,-2.06096735234555));
#7784=CARTESIAN_POINT('Ctrl Pts',(3.53586144539942,1.24572779455031,-2.06044500215379));
#7785=CARTESIAN_POINT('Ctrl Pts',(3.52463231606024,1.23156506551814,-2.05929092797132));
#7786=CARTESIAN_POINT('Ctrl Pts',(3.51855862899044,1.22378675362338,-2.05865851256569));
#7787=CARTESIAN_POINT('Ctrl Pts',(3.49736679797947,1.19622811540705,-2.05642257773849));
#7788=CARTESIAN_POINT('Ctrl Pts',(3.48256200104205,1.17621081724702,-2.05480694112109));
#7789=CARTESIAN_POINT('Ctrl Pts',(3.38419683273877,1.03786990551446,-2.04369318222381));
#7790=CARTESIAN_POINT('Ctrl Pts',(3.31338063896541,0.911046378908459,-2.03371244814949));
#7791=CARTESIAN_POINT('Ctrl Pts',(3.22229970809843,0.695916960728751,-2.01742803487771));
#7792=CARTESIAN_POINT('Ctrl Pts',(3.19317253352785,0.611906067753148,-2.01122440863533));
#7793=CARTESIAN_POINT('Ctrl Pts',(3.16276392903024,0.500721223268661,-2.00340107121701));
#7794=CARTESIAN_POINT('Ctrl Pts',(3.15629501476564,0.475075015445877,-2.00162285903775));
#7795=CARTESIAN_POINT('Ctrl Pts',(3.14636441778663,0.432119908282408,-1.99869625141013));
#7796=CARTESIAN_POINT('Ctrl Pts',(3.1426191046834,0.414880613727094,-1.99753545711134));
#7797=CARTESIAN_POINT('Ctrl Pts',(3.13776063432445,0.390994465850365,-1.99594813206982));
#7798=CARTESIAN_POINT('Ctrl Pts',(3.13645184116614,0.384388852052085,-1.99551137597878));
#7799=CARTESIAN_POINT('Ctrl Pts',(3.13429550657772,0.373208948657815,-1.99477605431741));
#7800=CARTESIAN_POINT('Ctrl Pts',(3.13343047766951,0.36863812826439,-1.99447651838746));
#7801=CARTESIAN_POINT('Ctrl Pts',(3.13180608524489,0.359887384887357,-1.99390520826274));
#7802=CARTESIAN_POINT('Ctrl Pts',(3.13104407657434,0.355708020473965,-1.99363328045654));
#7803=CARTESIAN_POINT('Ctrl Pts',(3.12925631544612,0.345722063083701,-1.99298570212458));
#7804=CARTESIAN_POINT('Ctrl Pts',(3.12824293888099,0.33991325359577,-1.99261074220388));
#7805=CARTESIAN_POINT('Ctrl Pts',(3.12471061916884,0.31912139028839,-1.99127454758547));
#7806=CARTESIAN_POINT('Ctrl Pts',(3.12233704012091,0.304113717187655,-1.99032106405391));
#7807=CARTESIAN_POINT('Ctrl Pts',(3.10023650338972,0.153222356487361,-1.98083133082115));
#7808=CARTESIAN_POINT('Ctrl Pts',(3.09441555649905,0.0156528983931978,-1.9729491464414));
#7809=CARTESIAN_POINT('Ctrl Pts',(3.11095558111533,-0.255527934421143,-1.95716955983568));
#7810=CARTESIAN_POINT('Ctrl Pts',(3.13265636811305,-0.388428686682874,-1.94930737402893));
#7811=CARTESIAN_POINT('Ctrl Pts',(3.17255310717885,-0.536754580247637,-1.93979670208566));
#7812=CARTESIAN_POINT('Ctrl Pts',(3.17783181584777,-0.555302859861251,-1.93859444779035));
#7813=CARTESIAN_POINT('Ctrl Pts',(3.18622671508031,-0.583254810269179,-1.93676173944622));
#7814=CARTESIAN_POINT('Ctrl Pts',(3.18914549201619,-0.592716938434015,-1.93613768237315));
#7815=CARTESIAN_POINT('Ctrl Pts',(3.19455757989457,-0.609809043564306,-1.93500359091428));
#7816=CARTESIAN_POINT('Ctrl Pts',(3.19702673977691,-0.617446491834715,-1.93449435433881));
#7817=CARTESIAN_POINT('Ctrl Pts',(3.20243272360087,-0.633829450706263,-1.93339656683139));
#7818=CARTESIAN_POINT('Ctrl Pts',(3.20538424765164,-0.642569878455398,-1.93280754321444));
#7819=CARTESIAN_POINT('Ctrl Pts',(3.2135099592179,-0.666093165803048,-1.9312130865811));
#7820=CARTESIAN_POINT('Ctrl Pts',(3.21879771252874,-0.680835831182161,-1.93020393475504));
#7821=CARTESIAN_POINT('Ctrl Pts',(3.24582499662956,-0.753486187097219,-1.92518081472669));
#7822=CARTESIAN_POINT('Ctrl Pts',(3.27007412107615,-0.810417744100414,-1.92108431788049));
#7823=CARTESIAN_POINT('Ctrl Pts',(3.37136604221896,-1.02056207300495,-1.9053431799186));
#7824=CARTESIAN_POINT('Ctrl Pts',(3.46540448874965,-1.16475156889398,-1.89317489703163));
#7825=CARTESIAN_POINT('Ctrl Pts',(3.61126322066226,-1.33561495660148,-1.87778408998894));
#7826=CARTESIAN_POINT('Ctrl Pts',(3.64744783066827,-1.37471854462379,-1.8741902155852));
#7827=CARTESIAN_POINT('Ctrl Pts',(3.69202977952111,-1.4191849397538,-1.87006213735716));
#7828=CARTESIAN_POINT('Ctrl Pts',(3.69895223745265,-1.42598939289992,-1.86942924761186));
#7829=CARTESIAN_POINT('Ctrl Pts',(3.70973042233325,-1.4364302548682,-1.86845666905404));
#7830=CARTESIAN_POINT('Ctrl Pts',(3.71355132129755,-1.44010217240138,-1.86811434165934));
#7831=CARTESIAN_POINT('Ctrl Pts',(3.72064609800737,-1.44686613883657,-1.86748329739197));
#7832=CARTESIAN_POINT('Ctrl Pts',(3.72391579635187,-1.44996231299428,-1.86719427223295));
#7833=CARTESIAN_POINT('Ctrl Pts',(3.73137520600397,-1.45697809280154,-1.86653894244609));
#7834=CARTESIAN_POINT('Ctrl Pts',(3.7355713568665,-1.46089070947657,-1.86617316777992));
#7835=CARTESIAN_POINT('Ctrl Pts',(3.74653973121813,-1.47102983953291,-1.86522431852028));
#7836=CARTESIAN_POINT('Ctrl Pts',(3.7533383393475,-1.47722778669541,-1.86464332121148));
#7837=CARTESIAN_POINT('Ctrl Pts',(3.7997186436483,-1.51892649567303,-1.86072582179016));
#7838=CARTESIAN_POINT('Ctrl Pts',(3.84066690019801,-1.55288280046686,-1.85749257820214));
#7839=CARTESIAN_POINT('Ctrl Pts',(4.01416773722097,-1.68541928329054,-1.84445891415586));
#7840=CARTESIAN_POINT('Ctrl Pts',(4.15735337543459,-1.76899002275367,-1.83516551565781));
#7841=CARTESIAN_POINT('Ctrl Pts',(4.37150485881377,-1.86060985445224,-1.82130162960991));
#7842=CARTESIAN_POINT('Ctrl Pts',(4.4351114643409,-1.88406759936948,-1.81719589091012));
#7843=CARTESIAN_POINT('Ctrl Pts',(4.514689932897,-1.90889273189382,-1.81201054531643));
#7844=CARTESIAN_POINT('Ctrl Pts',(4.52964998710048,-1.91336757717838,-1.81103379246082));
#7845=CARTESIAN_POINT('Ctrl Pts',(4.55343300755407,-1.92017837492005,-1.80947722474925));
#7846=CARTESIAN_POINT('Ctrl Pts',(4.5622223209512,-1.9226302614049,-1.80890117000283));
#7847=CARTESIAN_POINT('Ctrl Pts',(4.5787846958186,-1.92712828600353,-1.80781401756826));
#7848=CARTESIAN_POINT('Ctrl Pts',(4.58655392695947,-1.92918792099368,-1.80730336745326));
#7849=CARTESIAN_POINT('Ctrl Pts',(4.60405957132796,-1.93371563660825,-1.80615114758416));
#7850=CARTESIAN_POINT('Ctrl Pts',(4.61380254885207,-1.93615723036723,-1.8055087409522));
#7851=CARTESIAN_POINT('Ctrl Pts',(4.63876496371416,-1.94221282325051,-1.80385977858443));
#7852=CARTESIAN_POINT('Ctrl Pts',(4.65400900234703,-1.94572151612302,-1.80284989303897));
#7853=CARTESIAN_POINT('Ctrl Pts',(4.75575495810615,-1.96788343394683,-1.79608881186536));
#7854=CARTESIAN_POINT('Ctrl Pts',(4.84336276102063,-1.98093962023899,-1.79016164913342));
#7855=CARTESIAN_POINT('Ctrl Pts',(5.07636325173751,-1.99995919140142,-1.77415134467348));
#7856=CARTESIAN_POINT('Ctrl Pts',(5.22203550746561,-1.99592101731892,-1.76386577138007));
#7857=CARTESIAN_POINT('Ctrl Pts',(5.41571564699917,-1.96924776649251,-1.75049664133769));
#7858=CARTESIAN_POINT('Ctrl Pts',(5.46518814609382,-1.96052057389863,-1.74711380444139));
#7859=CARTESIAN_POINT('Ctrl Pts',(5.52363060481675,-1.94791889019578,-1.74319537663327));
#7860=CARTESIAN_POINT('Ctrl Pts',(5.53296407946433,-1.94583601019851,-1.7425719883546));
#7861=CARTESIAN_POINT('Ctrl Pts',(5.54741582043407,-1.94250164477213,-1.74161085337273));
#7862=CARTESIAN_POINT('Ctrl Pts',(5.55254456570101,-1.94129690053478,-1.74127056308892));
#7863=CARTESIAN_POINT('Ctrl Pts',(5.56205137523225,-1.93902396831564,-1.74064136100771));
#7864=CARTESIAN_POINT('Ctrl Pts',(5.56643056560525,-1.93796127077238,-1.74035215603611));
#7865=CARTESIAN_POINT('Ctrl Pts',(5.57641805286127,-1.93550174124016,-1.73969397788211));
#7866=CARTESIAN_POINT('Ctrl Pts',(5.58202390221554,-1.9340953707264,-1.7393255537349));
#7867=CARTESIAN_POINT('Ctrl Pts',(5.59667332082039,-1.93035243916039,-1.73836521013965));
#7868=CARTESIAN_POINT('Ctrl Pts',(5.60570685154834,-1.92797665703044,-1.73777545140949));
#7869=CARTESIAN_POINT('Ctrl Pts',(5.66928811630474,-1.91077665271845,-1.73363955515462));
#7870=CARTESIAN_POINT('Ctrl Pts',(5.723206173322,-1.89370168054198,-1.73021025284902));
#7871=CARTESIAN_POINT('Ctrl Pts',(5.92859742999109,-1.81891321859054,-1.71719443510743));
#7872=CARTESIAN_POINT('Ctrl Pts',(6.07354317976386,-1.74512131857496,-1.70806266097327));
#7873=CARTESIAN_POINT('Ctrl Pts',(6.26378675584202,-1.61701888855633,-1.69440764811976));
#7874=CARTESIAN_POINT('Ctrl Pts',(6.31765998583622,-1.5766379838887,-1.69032921642944));
#7875=CARTESIAN_POINT('Ctrl Pts',(6.38136792341492,-1.52364995974087,-1.68517456440074));
#7876=CARTESIAN_POINT('Ctrl Pts',(6.3932319680045,-1.5135446939177,-1.68419969724806));
#7877=CARTESIAN_POINT('Ctrl Pts',(6.41184789078608,-1.49730826676337,-1.682645447522));
#7878=CARTESIAN_POINT('Ctrl Pts',(6.41867837945663,-1.49126789487776,-1.6820698056457));
#7879=CARTESIAN_POINT('Ctrl Pts',(6.43145214793448,-1.47981470443325,-1.68098300636625));
#7880=CARTESIAN_POINT('Ctrl Pts',(6.43740460633235,-1.47441236103352,-1.68047229334903));
#7881=CARTESIAN_POINT('Ctrl Pts',(6.45072836084524,-1.46217227783025,-1.6793193617295));
#7882=CARTESIAN_POINT('Ctrl Pts',(6.45808089670971,-1.4553145277299,-1.67867630187591));
#7883=CARTESIAN_POINT('Ctrl Pts',(6.47676319871346,-1.43762344920925,-1.67702454319768));
#7884=CARTESIAN_POINT('Ctrl Pts',(6.48801751123237,-1.42671178243116,-1.67601249533346));
#7885=CARTESIAN_POINT('Ctrl Pts',(6.56262196859957,-1.35265298315237,-1.66918683263692));
#7886=CARTESIAN_POINT('Ctrl Pts',(6.62178284007282,-1.28544769403604,-1.66319325655863));
#7887=CARTESIAN_POINT('Ctrl Pts',(6.75564430867713,-1.11103749073305,-1.64812929812363));
#7888=CARTESIAN_POINT('Ctrl Pts',(6.82471357757324,-1.00003481566623,-1.63893001010521));
#7889=CARTESIAN_POINT('Ctrl Pts',(6.91039308217543,-0.826498102702352,-1.62560066827608));
#7890=CARTESIAN_POINT('Ctrl Pts',(6.93563541288106,-0.768605823072363,-1.62131707211403));
#7891=CARTESIAN_POINT('Ctrl Pts',(6.96168395391258,-0.700171759922608,-1.61651294717067));
#7892=CARTESIAN_POINT('Ctrl Pts',(6.96520424847747,-0.690707824548839,-1.61585421118863));
#7893=CARTESIAN_POINT('Ctrl Pts',(6.97049074793894,-0.676158482769902,-1.6148505683007));
#7894=CARTESIAN_POINT('Ctrl Pts',(6.9723084227119,-0.671092142249585,-1.61450275690487));
#7895=CARTESIAN_POINT('Ctrl Pts',(6.97560706736833,-0.661779531517981,-1.61386658392977));
#7896=CARTESIAN_POINT('Ctrl Pts',(6.97709418323862,-0.657535617341168,-1.61357787387638));
#7897=CARTESIAN_POINT('Ctrl Pts',(6.98041169243418,-0.647964562360384,-1.61292945202371));
#7898=CARTESIAN_POINT('Ctrl Pts',(6.98223387915297,-0.642634683939797,-1.61257022284331));
#7899=CARTESIAN_POINT('Ctrl Pts',(6.98753257154999,-0.626918902005126,-1.61151626510544));
#7900=CARTESIAN_POINT('Ctrl Pts',(6.99094621294328,-0.616511806128984,-1.61082508698636));
#7901=CARTESIAN_POINT('Ctrl Pts',(7.0219567838781,-0.519273405415327,-1.60442530062435));
#7902=CARTESIAN_POINT('Ctrl Pts',(7.04366363410773,-0.430663230940203,-1.59902224504291));
#7903=CARTESIAN_POINT('Ctrl Pts',(7.07867992308661,-0.228763448657466,-1.58704350817181));
#7904=CARTESIAN_POINT('Ctrl Pts',(7.08849541672183,-0.1152024391642,-1.58052419577023));
#7905=CARTESIAN_POINT('Ctrl Pts',(7.08857698602155,-0.000949408941870256,
-1.57376499307923));
#7906=CARTESIAN_POINT('Ctrl Pts',(7.08857715545312,-0.000474703094148514,
-1.5737369062833));
#7907=CARTESIAN_POINT('Ctrl Pts',(7.08857715545311,2.4467182997506E-11,
-1.57370881642439));
#7908=CARTESIAN_POINT('Origin',(5.09382715545311,0.,-6.77268258743872));
#7909=CARTESIAN_POINT('',(7.0885771212009,0.000270376244464336,-0.616403823242141));
#7910=CARTESIAN_POINT('',(7.08857666516212,0.0013985762946109,-0.772682587389958));
#7911=CARTESIAN_POINT('',(7.08857715545311,8.3550772080578E-14,-6.77268258743872));
#7912=CARTESIAN_POINT('Ctrl Pts',(7.08857709145056,0.000505309959526276,
-0.616403784479595));
#7913=CARTESIAN_POINT('Ctrl Pts',(7.08858289021834,-0.0223857719132102,
-0.617835630335221));
#7914=CARTESIAN_POINT('Ctrl Pts',(7.08819465309331,-0.0452765254613356,
-0.619248452783894));
#7915=CARTESIAN_POINT('Ctrl Pts',(7.08480907112761,-0.144304803472926,-0.625297633396242));
#7916=CARTESIAN_POINT('Ctrl Pts',(7.07784471547868,-0.220247985752777,-0.629777142771891));
#7917=CARTESIAN_POINT('Ctrl Pts',(7.05553837196678,-0.369106108127607,-0.638549028210189));
#7918=CARTESIAN_POINT('Ctrl Pts',(7.04042698139936,-0.441926830394387,-0.642836821697343));
#7919=CARTESIAN_POINT('Ctrl Pts',(6.99648402095372,-0.60679474210903,-0.652812289300294));
#7920=CARTESIAN_POINT('Ctrl Pts',(6.96497628648473,-0.697926019428036,-0.658529303843982));
#7921=CARTESIAN_POINT('Ctrl Pts',(6.91780763715039,-0.807878715294661,-0.665904141088645));
#7922=CARTESIAN_POINT('Ctrl Pts',(6.90822598185459,-0.829174073519144,-0.667355249116568));
#7923=CARTESIAN_POINT('Ctrl Pts',(6.89371739824139,-0.859963309400044,-0.669489014208158));
#7924=CARTESIAN_POINT('Ctrl Pts',(6.88908423477748,-0.869594038404518,-0.670161617281624));
#7925=CARTESIAN_POINT('Ctrl Pts',(6.88079755904406,-0.886470632540912,-0.671349614697471));
#7926=CARTESIAN_POINT('Ctrl Pts',(6.87717677573109,-0.893732361705636,-0.671863866204003));
#7927=CARTESIAN_POINT('Ctrl Pts',(6.86954763597928,-0.908802161267996,-0.672937577918472));
#7928=CARTESIAN_POINT('Ctrl Pts',(6.86553185883164,-0.916606258581189,-0.673497289044717));
#7929=CARTESIAN_POINT('Ctrl Pts',(6.85496437049203,-0.936813769660552,-0.674956291037723));
#7930=CARTESIAN_POINT('Ctrl Pts',(6.84833318420155,-0.94917485622856,-0.675858361531553));
#7931=CARTESIAN_POINT('Ctrl Pts',(6.82066760771554,-0.999465185523764,-0.679568527353132));
#7932=CARTESIAN_POINT('Ctrl Pts',(6.79853059049359,-1.03677110385418,-0.682415467955409));
#7933=CARTESIAN_POINT('Ctrl Pts',(6.68291248507604,-1.21788772898224,-0.696724198763139));
#7934=CARTESIAN_POINT('Ctrl Pts',(6.57237720829435,-1.34993124987602,-0.708811086967108));
#7935=CARTESIAN_POINT('Ctrl Pts',(6.40931332786564,-1.50035434560631,-0.724160611262132));
#7936=CARTESIAN_POINT('Ctrl Pts',(6.370989149762,-1.53310956880177,-0.727615733405562));
#7937=CARTESIAN_POINT('Ctrl Pts',(6.31681996805741,-1.57596471094612,-0.732255104929704));
#7938=CARTESIAN_POINT('Ctrl Pts',(6.30201430555295,-1.58734371020412,-0.733499377030884));
#7939=CARTESIAN_POINT('Ctrl Pts',(6.27950939233213,-1.60414268403876,-0.7353527061248));
#7940=CARTESIAN_POINT('Ctrl Pts',(6.27192838417006,-1.60971849104384,-0.73597066999277));
#7941=CARTESIAN_POINT('Ctrl Pts',(6.25955657932952,-1.61868369494767,-0.736968526545846));
#7942=CARTESIAN_POINT('Ctrl Pts',(6.25478988437308,-1.62210589607492,-0.737350455694226));
#7943=CARTESIAN_POINT('Ctrl Pts',(6.24562545066598,-1.62862431961302,-0.738079805786516));
#7944=CARTESIAN_POINT('Ctrl Pts',(6.24123016227255,-1.63172388254662,-0.738427443253408));
#7945=CARTESIAN_POINT('Ctrl Pts',(6.23679918682208,-1.63482185537315,-0.738775693026422));
#7946=CARTESIAN_POINT('Ctrl Pts',(6.23677604366833,-1.63483803547171,-0.738777511887826));
#7947=CARTESIAN_POINT('Ctrl Pts',(6.23673437116238,-1.63486716869928,-0.738780786894967));
#7948=CARTESIAN_POINT('Ctrl Pts',(6.23671584186986,-1.63488012204924,-0.738782243057715));
#7949=CARTESIAN_POINT('Ctrl Pts',(6.23667831977713,-1.63490635182576,-0.738785191730456));
#7950=CARTESIAN_POINT('Ctrl Pts',(6.23665932700194,-1.63491962821111,-0.738786684236524));
#7951=CARTESIAN_POINT('Ctrl Pts',(6.23662086078775,-1.63494651597904,-0.738789706938133));
#7952=CARTESIAN_POINT('Ctrl Pts',(6.23660138737839,-1.63496012731567,-0.73879123712926));
#7953=CARTESIAN_POINT('Ctrl Pts',(6.23656194194624,-1.63498769745592,-0.738794336605116));
#7954=CARTESIAN_POINT('Ctrl Pts',(6.23654196988223,-1.63500165626153,-0.738795905890866));
#7955=CARTESIAN_POINT('Ctrl Pts',(6.23650150820266,-1.63502993449456,-0.73879908503728));
#7956=CARTESIAN_POINT('Ctrl Pts',(6.23648101859543,-1.63504425388758,-0.738800694894928));
#7957=CARTESIAN_POINT('Ctrl Pts',(6.2364395019224,-1.63507326712108,-0.738803956742057));
#7958=CARTESIAN_POINT('Ctrl Pts',(6.23641847481323,-1.63508796096141,-0.738805608732427));
#7959=CARTESIAN_POINT('Ctrl Pts',(6.23637586214765,-1.63511773766419,-0.738808956486331));
#7960=CARTESIAN_POINT('Ctrl Pts',(6.23635427657312,-1.63513282050684,-0.738810652248604));
#7961=CARTESIAN_POINT('Ctrl Pts',(6.23631052481319,-1.63516339060256,-0.738814089279339));
#7962=CARTESIAN_POINT('Ctrl Pts',(6.23628835865227,-1.63517887780387,-0.738815830543013));
#7963=CARTESIAN_POINT('Ctrl Pts',(6.23624342236974,-1.63521027282604,-0.738819360402095));
#7964=CARTESIAN_POINT('Ctrl Pts',(6.23622065225917,-1.63522618060217,-0.738821148993577));
#7965=CARTESIAN_POINT('Ctrl Pts',(6.23617448348139,-1.63525843384503,-0.73882477543099));
#7966=CARTESIAN_POINT('Ctrl Pts',(6.23615108475217,-1.63527477931552,-0.73882661327852));
#7967=CARTESIAN_POINT('Ctrl Pts',(6.23610363268735,-1.63530792602438,-0.738830340264159));
#7968=CARTESIAN_POINT('Ctrl Pts',(6.23607957932842,-1.63532472723671,-0.738832229400598));
#7969=CARTESIAN_POINT('Ctrl Pts',(6.23603079044056,-1.63535880455384,-0.73883606111824));
#7970=CARTESIAN_POINT('Ctrl Pts',(6.23600605488848,-1.63537608062944,-0.738838003697509));
#7971=CARTESIAN_POINT('Ctrl Pts',(6.235955872445,-1.63541112790815,-0.738841944580185));
#7972=CARTESIAN_POINT('Ctrl Pts',(6.23593042553645,-1.63542889907459,-0.738843942880916));
#7973=CARTESIAN_POINT('Ctrl Pts',(6.23587878947609,-1.63546495796937,-0.738847997621108));
#7974=CARTESIAN_POINT('Ctrl Pts',(6.2358526003056,-1.63548324565853,-0.738850054057717));
#7975=CARTESIAN_POINT('Ctrl Pts',(6.23224338193742,-1.63800340513623,-0.739133447888702));
#7976=CARTESIAN_POINT('Ctrl Pts',(6.22865219236113,-1.64049346119307,-0.73941396923231));
#7977=CARTESIAN_POINT('Ctrl Pts',(6.22039429054586,-1.64617922520578,-0.740055714979887));
#7978=CARTESIAN_POINT('Ctrl Pts',(6.21572215522225,-1.64936689755544,-0.740416398428976));
#7979=CARTESIAN_POINT('Ctrl Pts',(6.20207763187366,-1.65859138668314,-0.741462964024277));
#7980=CARTESIAN_POINT('Ctrl Pts',(6.19306946809851,-1.66457527820847,-0.742145428951207));
#7981=CARTESIAN_POINT('Ctrl Pts',(6.10291374198274,-1.72341234507652,-0.748896450113127));
#7982=CARTESIAN_POINT('Ctrl Pts',(6.0180563434217,-1.77037040443351,-0.7546188859221));
#7983=CARTESIAN_POINT('Ctrl Pts',(5.81388476642289,-1.86465390604705,-0.767741134133508));
#7984=CARTESIAN_POINT('Ctrl Pts',(5.69276565915337,-1.90701040605596,-0.77507228147667));
#7985=CARTESIAN_POINT('Ctrl Pts',(5.50948168052885,-1.95190716769005,-0.786353968874066));
#7986=CARTESIAN_POINT('Ctrl Pts',(5.44991580250582,-1.96364713573061,-0.790044347807438));
#7987=CARTESIAN_POINT('Ctrl Pts',(5.37496133098747,-1.97489738447856,-0.794762200590383));
#7988=CARTESIAN_POINT('Ctrl Pts',(5.35998651766781,-1.97697123854038,-0.795708329606422));
#7989=CARTESIAN_POINT('Ctrl Pts',(5.33604562990981,-1.98000986405481,-0.797227248428666));
#7990=CARTESIAN_POINT('Ctrl Pts',(5.32709389129463,-1.98108441939477,-0.797796588101359));
#7991=CARTESIAN_POINT('Ctrl Pts',(5.31013205160602,-1.98300394012794,-0.798878159441434));
#7992=CARTESIAN_POINT('Ctrl Pts',(5.30212349622851,-1.98386115088095,-0.799389996078179));
#7993=CARTESIAN_POINT('Ctrl Pts',(5.28394466167901,-1.98569566753748,-0.800554581853837));
#7994=CARTESIAN_POINT('Ctrl Pts',(5.27377168756263,-1.98664337746271,-0.801208243244641));
#7995=CARTESIAN_POINT('Ctrl Pts',(5.2474376854137,-1.98889271569778,-0.802905570964789));
#7996=CARTESIAN_POINT('Ctrl Pts',(5.23126752185967,-1.99007551351617,-0.803952906813853));
#7997=CARTESIAN_POINT('Ctrl Pts',(5.08527100454034,-1.99896687370866,-0.8134571266548));
#7998=CARTESIAN_POINT('Ctrl Pts',(4.95501901233134,-1.99415713900583,-0.822310405395853));
#7999=CARTESIAN_POINT('Ctrl Pts',(4.73420610133288,-1.96425946123062,-0.837789554167223));
#8000=CARTESIAN_POINT('Ctrl Pts',(4.64320939007224,-1.9454013923649,-0.844300937635326));
#8001=CARTESIAN_POINT('Ctrl Pts',(4.51534860304006,-1.90944760851642,-0.853431311364357));
#8002=CARTESIAN_POINT('Ctrl Pts',(4.47717342355976,-1.89746308983248,-0.856153783391403));
#8003=CARTESIAN_POINT('Ctrl Pts',(4.41688694311996,-1.87652513749285,-0.860421870190493));
#8004=CARTESIAN_POINT('Ctrl Pts',(4.39453208902037,-1.86830971026244,-0.861997464657784));
#8005=CARTESIAN_POINT('Ctrl Pts',(4.36529154864434,-1.85696537537849,-0.864044174040803));
#8006=CARTESIAN_POINT('Ctrl Pts',(4.35826994395572,-1.85419527794546,-0.864534563995572));
#8007=CARTESIAN_POINT('Ctrl Pts',(4.34678634033727,-1.84958937573845,-0.865334589709168));
#8008=CARTESIAN_POINT('Ctrl Pts',(4.34231505483757,-1.8477771516406,-0.865645592455148));
#8009=CARTESIAN_POINT('Ctrl Pts',(4.33359241145023,-1.84420494172435,-0.866251265583746));
#8010=CARTESIAN_POINT('Ctrl Pts',(4.3293405130243,-1.8424464462249,-0.866546017023707));
#8011=CARTESIAN_POINT('Ctrl Pts',(4.31890270636355,-1.83808723648958,-0.867268477769702));
#8012=CARTESIAN_POINT('Ctrl Pts',(4.31272369152793,-1.83546995956914,-0.86769520027713));
#8013=CARTESIAN_POINT('Ctrl Pts',(4.29161078623088,-1.82640113248664,-0.869150342559267));
#8014=CARTESIAN_POINT('Ctrl Pts',(4.27674221285872,-1.81979791078204,-0.87017010189741));
#8015=CARTESIAN_POINT('Ctrl Pts',(4.17093278136729,-1.77124897625112,-0.877402555868397));
#8016=CARTESIAN_POINT('Ctrl Pts',(4.08317247633702,-1.72268368726434,-0.883275021406064));
#8017=CARTESIAN_POINT('Ctrl Pts',(3.93013555056186,-1.62225692499831,-0.893925138837197));
#8018=CARTESIAN_POINT('Ctrl Pts',(3.86374935412762,-1.572515177416,-0.898706348328159));
#8019=CARTESIAN_POINT('Ctrl Pts',(3.73728472955712,-1.4648366582771,-0.908472411864932));
#8020=CARTESIAN_POINT('Ctrl Pts',(3.67736367815897,-1.40697643654294,-0.913448834056087));
#8021=CARTESIAN_POINT('Ctrl Pts',(3.60660699495583,-1.32953902324299,-0.919926233545728));
#8022=CARTESIAN_POINT('Ctrl Pts',(3.59224170212754,-1.31329314680827,-0.921275559929294));
#8023=CARTESIAN_POINT('Ctrl Pts',(3.57139900333033,-1.28893279253484,-0.923286700333308));
#8024=CARTESIAN_POINT('Ctrl Pts',(3.56471518925752,-1.28099641309917,-0.923940052399901));
#8025=CARTESIAN_POINT('Ctrl Pts',(3.55294200233535,-1.26679346083781,-0.925106207113582));
#8026=CARTESIAN_POINT('Ctrl Pts',(3.54782814494878,-1.26054741438958,-0.925618004417759));
#8027=CARTESIAN_POINT('Ctrl Pts',(3.53713937934953,-1.24732931390649,-0.926698997964977));
#8028=CARTESIAN_POINT('Ctrl Pts',(3.53157309122741,-1.24035054889988,-0.927268523058301));
#8029=CARTESIAN_POINT('Ctrl Pts',(3.5169581783219,-1.2217725679385,-0.928781604221853));
#8030=CARTESIAN_POINT('Ctrl Pts',(3.50799084127706,-1.2101103851649,-0.929728334851506));
#8031=CARTESIAN_POINT('Ctrl Pts',(3.46940301769535,-1.15876063929167,-0.933884330608955));
#8032=CARTESIAN_POINT('Ctrl Pts',(3.44113950433593,-1.11807996807281,-0.937145132506772));
#8033=CARTESIAN_POINT('Ctrl Pts',(3.33526818861873,-0.952897711911929,-0.950271567276726));
#8034=CARTESIAN_POINT('Ctrl Pts',(3.2699876569743,-0.82106153185355,-0.960545422710943));
#8035=CARTESIAN_POINT('Ctrl Pts',(3.19143779420518,-0.605620590632464,-0.976488158561092));
#8036=CARTESIAN_POINT('Ctrl Pts',(3.16797287025663,-0.526260065823266,-0.982184617951813));
#8037=CARTESIAN_POINT('Ctrl Pts',(3.14590220465467,-0.429971147437003,-0.988728424216045));
#8038=CARTESIAN_POINT('Ctrl Pts',(3.14249496353832,-0.41423365126618,-0.989786334341946));
#8039=CARTESIAN_POINT('Ctrl Pts',(3.13798112874736,-0.392091912257889,-0.991256882777223));
#8040=CARTESIAN_POINT('Ctrl Pts',(3.13671480103206,-0.385721379823161,-0.991677916204127));
#8041=CARTESIAN_POINT('Ctrl Pts',(3.13460354167175,-0.374822110741027,-0.992394596106027));
#8042=CARTESIAN_POINT('Ctrl Pts',(3.13374314671583,-0.370296454061504,-0.992691102399556));
#8043=CARTESIAN_POINT('Ctrl Pts',(3.1319987438127,-0.360944482072323,-0.99330153966421));
#8044=CARTESIAN_POINT('Ctrl Pts',(3.13111685651705,-0.356117845053312,-0.993615351665187));
#8045=CARTESIAN_POINT('Ctrl Pts',(3.12885819148717,-0.343492712574617,-0.994433072608047));
#8046=CARTESIAN_POINT('Ctrl Pts',(3.12751001162107,-0.335689093970517,-0.994935397011909));
#8047=CARTESIAN_POINT('Ctrl Pts',(3.12216709753426,-0.303625843306616,-0.996987343730424));
#8048=CARTESIAN_POINT('Ctrl Pts',(3.11857437746895,-0.279300247551327,-0.998515989308374));
#8049=CARTESIAN_POINT('Ctrl Pts',(3.09813378656615,-0.120659712985837,-1.00833899078208));
#8050=CARTESIAN_POINT('Ctrl Pts',(3.09454380485881,0.0150220097502235,-1.01607927461657));
#8051=CARTESIAN_POINT('Ctrl Pts',(3.11113602919546,0.23499569193905,-1.02890952578856));
#8052=CARTESIAN_POINT('Ctrl Pts',(3.12298101761858,0.319454110522624,-1.03390087217809));
#8053=CARTESIAN_POINT('Ctrl Pts',(3.14989194620357,0.449946448848493,-1.04193752356205));
#8054=CARTESIAN_POINT('Ctrl Pts',(3.1612921083441,0.496632290651053,-1.04487856168617));
#8055=CARTESIAN_POINT('Ctrl Pts',(3.17818194593755,0.556352078378552,-1.04874765643286));
#8056=CARTESIAN_POINT('Ctrl Pts',(3.18214028745376,0.569804797047334,-1.04962630489286));
#8057=CARTESIAN_POINT('Ctrl Pts',(3.18880586394903,0.59160667258499,-1.05106230161777));
#8058=CARTESIAN_POINT('Ctrl Pts',(3.19142698840851,0.599981813544971,-1.05161684362798));
#8059=CARTESIAN_POINT('Ctrl Pts',(3.19657800280133,0.616067418186978,-1.05268764560082));
#8060=CARTESIAN_POINT('Ctrl Pts',(3.19909985085554,0.6237802890608,-1.0532036334809));
#8061=CARTESIAN_POINT('Ctrl Pts',(3.20499532383959,0.641445478869986,-1.05439139206596));
#8062=CARTESIAN_POINT('Ctrl Pts',(3.20840065038579,0.651386887727188,-1.05506419305756));
#8063=CARTESIAN_POINT('Ctrl Pts',(3.21922973981671,0.682204525022113,-1.05716369235184));
#8064=CARTESIAN_POINT('Ctrl Pts',(3.22692268027671,0.702983712366555,-1.05859921375342));
#8065=CARTESIAN_POINT('Ctrl Pts',(3.29808975885858,0.885798401157605,-1.07141079859375));
#8066=CARTESIAN_POINT('Ctrl Pts',(3.382158903225,1.0389797366191,-1.08351978686854));
#8067=CARTESIAN_POINT('Ctrl Pts',(3.54302532713859,1.25844160301574,-1.10246767441928));
#8068=CARTESIAN_POINT('Ctrl Pts',(3.60682335832631,1.33322380363297,-1.1092557686333));
#8069=CARTESIAN_POINT('Ctrl Pts',(3.68421842089496,1.41144304985929,-1.11649788076805));
#8070=CARTESIAN_POINT('Ctrl Pts',(3.69263681147172,1.41980065636516,-1.1172735795204));
#8071=CARTESIAN_POINT('Ctrl Pts',(3.70524041403133,1.43209196500548,-1.11841652141854));
#8072=CARTESIAN_POINT('Ctrl Pts',(3.70936868594647,1.4360833133506,-1.11878800935537));
#8073=CARTESIAN_POINT('Ctrl Pts',(3.71676530255033,1.4431730652731,-1.11944839223463));
#8074=CARTESIAN_POINT('Ctrl Pts',(3.72002695427016,1.44627827599345,-1.11973780361887));
#8075=CARTESIAN_POINT('Ctrl Pts',(3.72714683685021,1.45301084339284,-1.12036565824509));
#8076=CARTESIAN_POINT('Ctrl Pts',(3.73100900188762,1.4566338888509,-1.12070377622699));
#8077=CARTESIAN_POINT('Ctrl Pts',(3.74178494652321,1.46666228368675,-1.12164051083259));
#8078=CARTESIAN_POINT('Ctrl Pts',(3.74872986912068,1.47303417736222,-1.12223666195639));
#8079=CARTESIAN_POINT('Ctrl Pts',(3.7868373953119,1.5075031848339,-1.12546857903114));
#8080=CARTESIAN_POINT('Ctrl Pts',(3.81883782178845,1.5346631071771,-1.12804092809379));
#8081=CARTESIAN_POINT('Ctrl Pts',(3.96703687127094,1.65260679335656,-1.13945616323681));
#8082=CARTESIAN_POINT('Ctrl Pts',(4.09223098340434,1.73135142873996,-1.14780307873569));
#8083=CARTESIAN_POINT('Ctrl Pts',(4.3031814276704,1.83342746495134,-1.1615581968844));
#8084=CARTESIAN_POINT('Ctrl Pts',(4.38377390548446,1.86611863538257,-1.16674303265909));
#8085=CARTESIAN_POINT('Ctrl Pts',(4.48727625842137,1.90042494222461,-1.17347280024468));
#8086=CARTESIAN_POINT('Ctrl Pts',(4.50843194597942,1.90704780738036,-1.17485159767248));
#8087=CARTESIAN_POINT('Ctrl Pts',(4.53973309882718,1.91627683446841,-1.17689831621412));
#8088=CARTESIAN_POINT('Ctrl Pts',(4.54979621094097,1.91915800668901,-1.17755732819381));
#8089=CARTESIAN_POINT('Ctrl Pts',(4.56767039414373,1.92412369045163,-1.17872985240924));
#8090=CARTESIAN_POINT('Ctrl Pts',(4.57547239340425,1.92624018522141,-1.17924231903356));
#8091=CARTESIAN_POINT('Ctrl Pts',(4.59187067673215,1.93058180380697,-1.18032091488799));
#8092=CARTESIAN_POINT('Ctrl Pts',(4.60046936607575,1.9327970651867,-1.18088734894532));
#8093=CARTESIAN_POINT('Ctrl Pts',(4.6231437700986,1.93847745487856,-1.18238340339468));
#8094=CARTESIAN_POINT('Ctrl Pts',(4.6372427574233,1.94184663695781,-1.18331607183031));
#8095=CARTESIAN_POINT('Ctrl Pts',(4.69764551290223,1.95558667036054,-1.1873229024814));
#8096=CARTESIAN_POINT('Ctrl Pts',(4.74427137312759,1.96445647619298,-1.19044412396938));
#8097=CARTESIAN_POINT('Ctrl Pts',(4.97599827618466,2.00002797374892,-1.20610505563317));
#8098=CARTESIAN_POINT('Ctrl Pts',(5.16389226027774,2.00226509918841,-1.21938695356209));
#8099=CARTESIAN_POINT('Ctrl Pts',(5.40345895116653,1.9713291085138,-1.23594900869008));
#8100=CARTESIAN_POINT('Ctrl Pts',(5.45731914213056,1.96211239430875,-1.23963791043293));
#8101=CARTESIAN_POINT('Ctrl Pts',(5.52028924153241,1.94865416293136,-1.24385993806747));
#8102=CARTESIAN_POINT('Ctrl Pts',(5.52982568748204,1.94654263938508,-1.2444968396957));
#8103=CARTESIAN_POINT('Ctrl Pts',(5.5445244597398,1.94317465032612,-1.24547424635385));
#8104=CARTESIAN_POINT('Ctrl Pts',(5.54969776346179,1.94196750026914,-1.24581743052318));
#8105=CARTESIAN_POINT('Ctrl Pts',(5.55924623704794,1.93969917973655,-1.24644926025576));
#8106=CARTESIAN_POINT('Ctrl Pts',(5.56362261719699,1.93864386987071,-1.24673822043001));
#8107=CARTESIAN_POINT('Ctrl Pts',(5.5735515309157,1.93621403878744,-1.24739240019901));
#8108=CARTESIAN_POINT('Ctrl Pts',(5.57910174357462,1.93483044644351,-1.24775709759942));
#8109=CARTESIAN_POINT('Ctrl Pts',(5.59350727074235,1.93117345858889,-1.24870128532219));
#8110=CARTESIAN_POINT('Ctrl Pts',(5.60235315908241,1.9288629956175,-1.24927873176008));
#8111=CARTESIAN_POINT('Ctrl Pts',(5.6615964053081,1.9129533284828,-1.25313222067828));
#8112=CARTESIAN_POINT('Ctrl Pts',(5.71146379575825,1.8974399502471,-1.2563087420089));
#8113=CARTESIAN_POINT('Ctrl Pts',(5.91719399177631,1.82446623421212,-1.26934999890745));
#8114=CARTESIAN_POINT('Ctrl Pts',(6.06617646748187,1.74961519986767,-1.27869161062462));
#8115=CARTESIAN_POINT('Ctrl Pts',(6.26056699817922,1.61936870403373,-1.29261768816255));
#8116=CARTESIAN_POINT('Ctrl Pts',(6.31499747994002,1.57872684182096,-1.2967313369423));
#8117=CARTESIAN_POINT('Ctrl Pts',(6.37927243981559,1.52541865754462,-1.30192557262718));
#8118=CARTESIAN_POINT('Ctrl Pts',(6.39118032738342,1.51530405707303,-1.30290286841909));
#8119=CARTESIAN_POINT('Ctrl Pts',(6.4098541705187,1.4990609585207,-1.30446010345531));
#8120=CARTESIAN_POINT('Ctrl Pts',(6.41669914279628,1.49302396577715,-1.30503627699238));
#8121=CARTESIAN_POINT('Ctrl Pts',(6.42949363124932,1.48158267652179,-1.30612353115639));
#8122=CARTESIAN_POINT('Ctrl Pts',(6.43545239999776,1.47618896556273,-1.30663416329348));
#8123=CARTESIAN_POINT('Ctrl Pts',(6.44878200613385,1.46397600546527,-1.30778617909207));
#8124=CARTESIAN_POINT('Ctrl Pts',(6.4561342330428,1.45713685432712,-1.3084283983776));
#8125=CARTESIAN_POINT('Ctrl Pts',(6.4748000680814,1.43950886356093,-1.3100765591874));
#8126=CARTESIAN_POINT('Ctrl Pts',(6.48603888442882,1.42864216386905,-1.31108582501924));
#8127=CARTESIAN_POINT('Ctrl Pts',(6.55983887813781,1.3555878169169,-1.31782808293402));
#8128=CARTESIAN_POINT('Ctrl Pts',(6.61833513760812,1.28944961857603,-1.32373588577135));
#8129=CARTESIAN_POINT('Ctrl Pts',(6.75268873949323,1.11557598102997,-1.33878255090068));
#8130=CARTESIAN_POINT('Ctrl Pts',(6.82262059997119,1.00379351305069,-1.34806102897913));
#8131=CARTESIAN_POINT('Ctrl Pts',(6.9091576394201,0.829223127540357,-1.36148163602892));
#8132=CARTESIAN_POINT('Ctrl Pts',(6.93456294866335,0.771186879097831,-1.36577905863849));
#8133=CARTESIAN_POINT('Ctrl Pts',(6.96077324543181,0.702596574505435,-1.37059660451248));
#8134=CARTESIAN_POINT('Ctrl Pts',(6.96430817313933,0.693130883840755,-1.37125578751839));
#8135=CARTESIAN_POINT('Ctrl Pts',(6.9696162664558,0.678580694983217,-1.37225996678204));
#8136=CARTESIAN_POINT('Ctrl Pts',(6.9714409626117,0.673515360906222,-1.37260787222532));
#8137=CARTESIAN_POINT('Ctrl Pts',(6.97475206747224,0.664205736124418,-1.37324413507345));
#8138=CARTESIAN_POINT('Ctrl Pts',(6.97624463054939,0.659963813251686,-1.37353284163636));
#8139=CARTESIAN_POINT('Ctrl Pts',(6.97957390216103,0.65039870659977,-1.37418115366984));
#8140=CARTESIAN_POINT('Ctrl Pts',(6.98140242061994,0.645072779197203,-1.37454027728808));
#8141=CARTESIAN_POINT('Ctrl Pts',(6.98671835366424,0.629372903894551,-1.37559363474468));
#8142=CARTESIAN_POINT('Ctrl Pts',(6.99014304056991,0.618977719301734,-1.37628432418162));
#8143=CARTESIAN_POINT('Ctrl Pts',(7.02046018163391,0.52434018555716,-1.38251562447046));
#8144=CARTESIAN_POINT('Ctrl Pts',(7.04181204608914,0.438413472640924,-1.3877686451868));
#8145=CARTESIAN_POINT('Ctrl Pts',(7.07805807749167,0.235844000376361,-1.39981019930376));
#8146=CARTESIAN_POINT('Ctrl Pts',(7.08849340272321,0.118748857292228,-1.4065260971332));
#8147=CARTESIAN_POINT('Ctrl Pts',(7.08857698811124,0.000943538781985227,
-1.41349835193204));
#8148=CARTESIAN_POINT('Ctrl Pts',(7.08857715545312,0.000471768043527199,
-1.41352627668663));
#8149=CARTESIAN_POINT('Ctrl Pts',(7.08857715545311,-2.35333930719797E-11,
-1.41355420449641));
#8150=CARTESIAN_POINT('Ctrl Pts',(7.08857715545311,2.4467182997506E-11,
-1.57370881642439));
#8151=CARTESIAN_POINT('Ctrl Pts',(7.08857715545217,0.0768861269152348,-1.56915919293977));
#8152=CARTESIAN_POINT('Ctrl Pts',(7.08413199193511,0.153700428581474,-1.56452529786783));
#8153=CARTESIAN_POINT('Ctrl Pts',(7.07351340899662,0.245154597534047,-1.55880772583754));
#8154=CARTESIAN_POINT('Ctrl Pts',(7.07158860242346,0.260226974266608,-1.55785898216073));
#8155=CARTESIAN_POINT('Ctrl Pts',(7.06812460139678,0.285088259280509,-1.55628274489061));
#8156=CARTESIAN_POINT('Ctrl Pts',(7.06668430205023,0.294890478106148,-1.5556583544683));
#8157=CARTESIAN_POINT('Ctrl Pts',(7.06394499566413,0.312614285930607,-1.55452390847148));
#8158=CARTESIAN_POINT('Ctrl Pts',(7.06267107243397,0.32053958193332,-1.55401465307066));
#8159=CARTESIAN_POINT('Ctrl Pts',(7.05983097275455,0.3375523453662,-1.55291710636448));
#8160=CARTESIAN_POINT('Ctrl Pts',(7.05824955151252,0.346637044575541,-1.55232834423656));
#8161=CARTESIAN_POINT('Ctrl Pts',(7.05374185745093,0.371510100853789,-1.55070885343642));
#8162=CARTESIAN_POINT('Ctrl Pts',(7.05068789766292,0.387274327601949,-1.54967411249181));
#8163=CARTESIAN_POINT('Ctrl Pts',(7.03228431834651,0.476489164352646,-1.54376946965414));
#8164=CARTESIAN_POINT('Ctrl Pts',(7.01299189755982,0.549055913182397,-1.53877529113696));
#8165=CARTESIAN_POINT('Ctrl Pts',(6.95814151957859,0.716680755396122,-1.52678713662946));
#8166=CARTESIAN_POINT('Ctrl Pts',(6.91932913515949,0.810455970617528,-1.51971877267814));
#8167=CARTESIAN_POINT('Ctrl Pts',(6.84845330252681,0.950476840054279,-1.50878147734263));
#8168=CARTESIAN_POINT('Ctrl Pts',(6.82127819641459,0.9990157641976,-1.50491521831595));
#8169=CARTESIAN_POINT('Ctrl Pts',(6.76423143520207,1.09160508115647,-1.49746161270735));
#8170=CARTESIAN_POINT('Ctrl Pts',(6.7345531732624,1.13572502132681,-1.49387246181544));
#8171=CARTESIAN_POINT('Ctrl Pts',(6.69771028153764,1.18603165721879,-1.48978059415843));
#8172=CARTESIAN_POINT('Ctrl Pts',(6.6922239255966,1.19341524498623,-1.48918005244011));
#8173=CARTESIAN_POINT('Ctrl Pts',(6.68323320448872,1.20534181265451,-1.48821040722493));
#8174=CARTESIAN_POINT('Ctrl Pts',(6.67976004357428,1.20990799253566,-1.48783926693516));
#8175=CARTESIAN_POINT('Ctrl Pts',(6.67352562192623,1.21803144237959,-1.48717925767719));
#8176=CARTESIAN_POINT('Ctrl Pts',(6.67077197394222,1.22159440092352,-1.48688987469165));
#8177=CARTESIAN_POINT('Ctrl Pts',(6.66475137993622,1.22933019446755,-1.48626179953753));
#8178=CARTESIAN_POINT('Ctrl Pts',(6.66147986550272,1.23349934265803,-1.48592343453841));
#8179=CARTESIAN_POINT('Ctrl Pts',(6.65216869559997,1.24526842120195,-1.48496847939245));
#8180=CARTESIAN_POINT('Ctrl Pts',(6.6460900253029,1.25283749484317,-1.48435457202789));
#8181=CARTESIAN_POINT('Ctrl Pts',(6.60629620498284,1.30165392837125,-1.48039463096743));
#8182=CARTESIAN_POINT('Ctrl Pts',(6.57099223478799,1.34158488252399,-1.47715263298696));
#8183=CARTESIAN_POINT('Ctrl Pts',(6.41537130766339,1.50399910773336,-1.46371744861686));
#8184=CARTESIAN_POINT('Ctrl Pts',(6.28111142856201,1.61209653390755,-1.45407869495032));
#8185=CARTESIAN_POINT('Ctrl Pts',(6.08209068898047,1.7338282404175,-1.44014883016587));
#8186=CARTESIAN_POINT('Ctrl Pts',(6.028062743396,1.76352712750665,-1.43640620186798));
#8187=CARTESIAN_POINT('Ctrl Pts',(5.958705569321,1.79756993727488,-1.43160165100466));
#8188=CARTESIAN_POINT('Ctrl Pts',(5.94458022224486,1.8042980761701,-1.43062324213204));
#8189=CARTESIAN_POINT('Ctrl Pts',(5.92200602842218,1.81472652333584,-1.429059074028));
#8190=CARTESIAN_POINT('Ctrl Pts',(5.91360795602271,1.81853568415618,-1.42847705489128));
#8191=CARTESIAN_POINT('Ctrl Pts',(5.89785086193264,1.82555138934413,-1.42738467039266));
#8192=CARTESIAN_POINT('Ctrl Pts',(5.89049828665048,1.82877202006165,-1.42687479811112));
#8193=CARTESIAN_POINT('Ctrl Pts',(5.87402799139166,1.83586828763527,-1.4257322298307));
#8194=CARTESIAN_POINT('Ctrl Pts',(5.86490048308439,1.83972053082239,-1.42509875680098));
#8195=CARTESIAN_POINT('Ctrl Pts',(5.83789964634047,1.85087993562018,-1.42322378419378));
#8196=CARTESIAN_POINT('Ctrl Pts',(5.81994889368163,1.85799558280552,-1.42197590918335));
#8197=CARTESIAN_POINT('Ctrl Pts',(5.6755575287839,1.91282003467045,-1.41192453448759));
#8198=CARTESIAN_POINT('Ctrl Pts',(5.54469266456362,1.94781890112191,-1.40269455013442));
#8199=CARTESIAN_POINT('Ctrl Pts',(5.27666430574581,1.99103028085902,-1.38380865480221));
#8200=CARTESIAN_POINT('Ctrl Pts',(5.14012811850766,1.99887286780517,-1.37420434704263));
#8201=CARTESIAN_POINT('Ctrl Pts',(4.98861217754417,1.99203165282899,-1.36416446514001));
#8202=CARTESIAN_POINT('Ctrl Pts',(4.97337988877494,1.99116869879459,-1.36316243091137));
#8203=CARTESIAN_POINT('Ctrl Pts',(4.9522659971156,1.98972934929157,-1.36178497725543));
#8204=CARTESIAN_POINT('Ctrl Pts',(4.94637525652777,1.9893014815796,-1.36140191287495));
#8205=CARTESIAN_POINT('Ctrl Pts',(4.93624824512703,1.98852068592968,-1.36074560910017));
#8206=CARTESIAN_POINT('Ctrl Pts',(4.93201108312698,1.98818037182525,-1.36047168450437));
#8207=CARTESIAN_POINT('Ctrl Pts',(4.92314158343221,1.98743946229763,-1.35989974558767));
#8208=CARTESIAN_POINT('Ctrl Pts',(4.91850951541889,1.98703621166551,-1.35960189032805));
#8209=CARTESIAN_POINT('Ctrl Pts',(4.90718444039631,1.98601038325817,-1.35887561680763));
#8210=CARTESIAN_POINT('Ctrl Pts',(4.90049301049568,1.98537015616635,-1.35844817305147));
#8211=CARTESIAN_POINT('Ctrl Pts',(4.87633352190744,1.98293530627907,-1.35691052482799));
#8212=CARTESIAN_POINT('Ctrl Pts',(4.85888552049683,1.98094381225378,-1.35581069808715));
#8213=CARTESIAN_POINT('Ctrl Pts',(4.81539197746638,1.97539674381059,-1.35309068693876));
#8214=CARTESIAN_POINT('Ctrl Pts',(4.78938555395295,1.9715562097802,-1.35148367924389));
#8215=CARTESIAN_POINT('Ctrl Pts',(4.67682236457926,1.95265270658149,-1.34458323424197));
#8216=CARTESIAN_POINT('Ctrl Pts',(4.5912322449369,1.93239393326732,-1.33947557748124));
#8217=CARTESIAN_POINT('Ctrl Pts',(4.36756250820291,1.86357913676258,-1.32588764687039));
#8218=CARTESIAN_POINT('Ctrl Pts',(4.23303702886595,1.80538691636256,-1.31742819370428));
#8219=CARTESIAN_POINT('Ctrl Pts',(4.08477931931321,1.72088673071914,-1.3069257333719));
#8220=CARTESIAN_POINT('Ctrl Pts',(4.06370496791276,1.7083550195488,-1.3054039281175));
#8221=CARTESIAN_POINT('Ctrl Pts',(4.03439120010911,1.69018415471465,-1.30324344087637));
#8222=CARTESIAN_POINT('Ctrl Pts',(4.02595441758008,1.68486641318354,-1.30261643818217));
#8223=CARTESIAN_POINT('Ctrl Pts',(4.01125659756604,1.67544757116724,-1.30151481735425));
#8224=CARTESIAN_POINT('Ctrl Pts',(4.00497805609663,1.67137404936516,-1.30104122217721));
#8225=CARTESIAN_POINT('Ctrl Pts',(3.99181301925058,1.66272690078038,-1.30004173497001));
#8226=CARTESIAN_POINT('Ctrl Pts',(3.98493174881525,1.65814561385241,-1.2995155636511));
#8227=CARTESIAN_POINT('Ctrl Pts',(3.96847528340446,1.64704127421749,-1.29824808889974));
#8228=CARTESIAN_POINT('Ctrl Pts',(3.95892814195743,1.64047737403499,-1.29750525856094));
#8229=CARTESIAN_POINT('Ctrl Pts',(3.92599092804313,1.61740707724775,-1.29491594113832));
#8230=CARTESIAN_POINT('Ctrl Pts',(3.90290031391413,1.60048124798541,-1.29305358628486));
#8231=CARTESIAN_POINT('Ctrl Pts',(3.76267341018936,1.49297740583364,-1.28144261947988));
#8232=CARTESIAN_POINT('Ctrl Pts',(3.65557942579559,1.3901008799441,-1.27119789647535));
#8233=CARTESIAN_POINT('Ctrl Pts',(3.49166330538878,1.19322961525116,-1.25333764453476));
#8234=CARTESIAN_POINT('Ctrl Pts',(3.42932548616171,1.10461062277575,-1.24580123940056));
#8235=CARTESIAN_POINT('Ctrl Pts',(3.36620987721488,0.997312367766644,-1.23754907466764));
#8236=CARTESIAN_POINT('Ctrl Pts',(3.35811526454825,0.98315700247315,-1.23647700619968));
#8237=CARTESIAN_POINT('Ctrl Pts',(3.34693245486155,0.963032490996198,-1.23497782209772));
#8238=CARTESIAN_POINT('Ctrl Pts',(3.3436996943103,0.957144997665118,-1.23454221011597));
#8239=CARTESIAN_POINT('Ctrl Pts',(3.33830197154852,0.947195899620492,-1.23381123320434));
#8240=CARTESIAN_POINT('Ctrl Pts',(3.33612123579191,0.943142961100182,-1.23351488844479));
#8241=CARTESIAN_POINT('Ctrl Pts',(3.33168408795248,0.934827594069914,-1.23290986155207));
#8242=CARTESIAN_POINT('Ctrl Pts',(3.32942907838012,0.930564478041992,-1.23260126692047));
#8243=CARTESIAN_POINT('Ctrl Pts',(3.32368825782938,0.919615515074339,-1.23181266332265));
#8244=CARTESIAN_POINT('Ctrl Pts',(3.3202248149079,0.912917934096015,-1.23133403597237));
#8245=CARTESIAN_POINT('Ctrl Pts',(3.30601302874139,0.885049121368304,-1.22935737611577));
#8246=CARTESIAN_POINT('Ctrl Pts',(3.29560463352925,0.863705492415834,-1.22787908323097));
#8247=CARTESIAN_POINT('Ctrl Pts',(3.26876210355763,0.806071796077251,-1.22396819964988));
#8248=CARTESIAN_POINT('Ctrl Pts',(3.25302918088304,0.769465654246573,-1.22156844859414));
#8249=CARTESIAN_POINT('Ctrl Pts',(3.20425498421416,0.645905397347893,-1.21366842706614));
#8250=CARTESIAN_POINT('Ctrl Pts',(3.17619772852972,0.557113830700254,-1.20831013083785));
#8251=CARTESIAN_POINT('Ctrl Pts',(3.12399340216493,0.340169798654947,-1.19534054034536));
#8252=CARTESIAN_POINT('Ctrl Pts',(3.10600567911421,0.210997357617773,-1.18769847724863));
#8253=CARTESIAN_POINT('Ctrl Pts',(3.10006439052321,0.0648093677771114,-1.17862522918925));
#8254=CARTESIAN_POINT('Ctrl Pts',(3.09960365997113,0.0486090833919524,-1.17761436914685));
#8255=CARTESIAN_POINT('Ctrl Pts',(3.09917444345262,0.0221916315012395,-1.17595640585021));
#8256=CARTESIAN_POINT('Ctrl Pts',(3.09908695771417,0.0119769489165365,-1.17531299946694));
#8257=CARTESIAN_POINT('Ctrl Pts',(3.0990708186893,-0.00629191974975199,
-1.17415791459135));
#8258=CARTESIAN_POINT('Ctrl Pts',(3.09911248332419,-0.0143459057394821,
-1.1736471708984));
#8259=CARTESIAN_POINT('Ctrl Pts',(3.09930417725768,-0.0314159464480813,
-1.17256136685666));
#8260=CARTESIAN_POINT('Ctrl Pts',(3.09946656891587,-0.0404316549372829,
-1.17198593282258));
#8261=CARTESIAN_POINT('Ctrl Pts',(3.10006494771478,-0.0645641103545041,
-1.17044027594198));
#8262=CARTESIAN_POINT('Ctrl Pts',(3.10061171914711,-0.0796772803540742,
-1.16946663079102));
#8263=CARTESIAN_POINT('Ctrl Pts',(3.10421717908372,-0.155470518225676,-1.1645542969945));
#8264=CARTESIAN_POINT('Ctrl Pts',(3.10987494328644,-0.215989034429837,-1.1605356946821));
#8265=CARTESIAN_POINT('Ctrl Pts',(3.13605033054297,-0.403244387221179,-1.1477952072643));
#8266=CARTESIAN_POINT('Ctrl Pts',(3.16603794446212,-0.528316267293695,-1.13882183741282));
#8267=CARTESIAN_POINT('Ctrl Pts',(3.23921550968878,-0.740766878977301,-1.12318184647927));
#8268=CARTESIAN_POINT('Ctrl Pts',(3.27717816630783,-0.829524407888211,-1.11652495514493));
#8269=CARTESIAN_POINT('Ctrl Pts',(3.32643997921539,-0.924927052015169,-1.10946783366581));
#8270=CARTESIAN_POINT('Ctrl Pts',(3.33154440861088,-0.934615972152766,-1.10875237788209));
#8271=CARTESIAN_POINT('Ctrl Pts',(3.33939471564807,-0.949223946216446,-1.10767614459492));
#8272=CARTESIAN_POINT('Ctrl Pts',(3.34208196589076,-0.954174029532902,-1.10731188177832));
#8273=CARTESIAN_POINT('Ctrl Pts',(3.34695239162603,-0.963055732733448,-1.10665917037015));
#8274=CARTESIAN_POINT('Ctrl Pts',(3.34912791731066,-0.966991393165042,-1.1063702559096));
#8275=CARTESIAN_POINT('Ctrl Pts',(3.35393676363011,-0.975621832643846,-1.10573739625538));
#8276=CARTESIAN_POINT('Ctrl Pts',(3.35657578132915,-0.980313317583523,-1.1053938180484));
#8277=CARTESIAN_POINT('Ctrl Pts',(3.36422023774594,-0.993775350464348,-1.10440904102709));
#8278=CARTESIAN_POINT('Ctrl Pts',(3.36927341407417,-1.00251879791121,-1.10377079679464));
#8279=CARTESIAN_POINT('Ctrl Pts',(3.40640526148438,-1.0656559356145,-1.09916906478161));
#8280=CARTESIAN_POINT('Ctrl Pts',(3.44098790230944,-1.11854340209923,-1.09535232297778));
#8281=CARTESIAN_POINT('Ctrl Pts',(3.55465984221424,-1.27556690800239,-1.08385579033966));
#8282=CARTESIAN_POINT('Ctrl Pts',(3.64151378687392,-1.37364317600236,-1.07641885075015));
#8283=CARTESIAN_POINT('Ctrl Pts',(3.80271151906069,-1.52315383809513,-1.06348609632469));
#8284=CARTESIAN_POINT('Ctrl Pts',(3.87206679725908,-1.57932768116212,-1.05814423095602));
#8285=CARTESIAN_POINT('Ctrl Pts',(3.95774707164088,-1.63969357409771,-1.05163967840722));
#8286=CARTESIAN_POINT('Ctrl Pts',(3.97065896306921,-1.64856488001505,-1.05066201580661));
#8287=CARTESIAN_POINT('Ctrl Pts',(3.99202457489852,-1.66287692411542,-1.04904769749925));
#8288=CARTESIAN_POINT('Ctrl Pts',(4.00041746196959,-1.66840757236939,-1.04841441565892));
#8289=CARTESIAN_POINT('Ctrl Pts',(4.01559687510943,-1.67824659639889,-1.04727041537831));
#8290=CARTESIAN_POINT('Ctrl Pts',(4.02236836621946,-1.68257785426699,-1.04676056007491));
#8291=CARTESIAN_POINT('Ctrl Pts',(4.03687831104672,-1.69173575980882,-1.04566896651476));
#8292=CARTESIAN_POINT('Ctrl Pts',(4.04462403627758,-1.69655048580351,-1.04508680495376));
#8293=CARTESIAN_POINT('Ctrl Pts',(4.06570181892477,-1.70945283786425,-1.04350396039319));
#8294=CARTESIAN_POINT('Ctrl Pts',(4.07909591372472,-1.71743739237585,-1.04249956294312));
#8295=CARTESIAN_POINT('Ctrl Pts',(4.15090163236803,-1.75910935462844,-1.03712140143012));
#8296=CARTESIAN_POINT('Ctrl Pts',(4.21089355240965,-1.78997227911487,-1.03264824053934));
#8297=CARTESIAN_POINT('Ctrl Pts',(4.42083251040441,-1.88485118200897,-1.01705864893429));
#8298=CARTESIAN_POINT('Ctrl Pts',(4.57699929103611,-1.93351094892902,-1.00551021381818));
#8299=CARTESIAN_POINT('Ctrl Pts',(4.79196343746431,-1.97255956546963,-0.990515375249305));
#8300=CARTESIAN_POINT('Ctrl Pts',(4.84701171775522,-1.98020107366046,-0.986758935272432));
#8301=CARTESIAN_POINT('Ctrl Pts',(4.91156957355505,-1.98642800863067,-0.98250196070733));
#8302=CARTESIAN_POINT('Ctrl Pts',(4.92083333916232,-1.98725620067313,-0.981894664825687));
#8303=CARTESIAN_POINT('Ctrl Pts',(4.93585077927576,-1.9884929697595,-0.980916309747214));
#8304=CARTESIAN_POINT('Ctrl Pts',(4.94160090304123,-1.98894142606119,-0.980543154998738));
#8305=CARTESIAN_POINT('Ctrl Pts',(4.95184614098072,-1.98969576870291,-0.979880974602804));
#8306=CARTESIAN_POINT('Ctrl Pts',(4.95634042094851,-1.99001137174198,-0.979591420901822));
#8307=CARTESIAN_POINT('Ctrl Pts',(4.96610099312964,-1.99066356655519,-0.978964596075611));
#8308=CARTESIAN_POINT('Ctrl Pts',(4.97136756076725,-1.99099448943703,-0.978627641186583));
#8309=CARTESIAN_POINT('Ctrl Pts',(4.98622151248584,-1.99186867009812,-0.977680694641381));
#8310=CARTESIAN_POINT('Ctrl Pts',(4.99581174823293,-1.99236361189293,-0.977073314857825));
#8311=CARTESIAN_POINT('Ctrl Pts',(5.05638700014822,-1.99505138702975,-0.973260051893567));
#8312=CARTESIAN_POINT('Ctrl Pts',(5.10744151684906,-1.99535646581558,-0.970149522679433));
#8313=CARTESIAN_POINT('Ctrl Pts',(5.30991937716985,-1.98879284262045,-0.958027869018999));
#8314=CARTESIAN_POINT('Ctrl Pts',(5.46033616239323,-1.96663921428979,-0.94946407076443));
#8315=CARTESIAN_POINT('Ctrl Pts',(5.68574676728199,-1.90665479757553,-0.935696227872132));
#8316=CARTESIAN_POINT('Ctrl Pts',(5.7633188714487,-1.88081893085974,-0.930784537706651));
#8317=CARTESIAN_POINT('Ctrl Pts',(5.85343180877563,-1.84452368324058,-0.924753862395435));
#8318=CARTESIAN_POINT('Ctrl Pts',(5.86771245360311,-1.83857781225466,-0.923788279759531));
#8319=CARTESIAN_POINT('Ctrl Pts',(5.8911007013813,-1.82851915019943,-0.922189862035545));
#8320=CARTESIAN_POINT('Ctrl Pts',(5.90024928284875,-1.82450287374515,-0.92156028653491));
#8321=CARTESIAN_POINT('Ctrl Pts',(5.91669834298389,-1.81713376065756,-0.920420291048438));
#8322=CARTESIAN_POINT('Ctrl Pts',(5.92400951614949,-1.81380521013281,-0.919910707966358));
#8323=CARTESIAN_POINT('Ctrl Pts',(5.93144163465702,-1.81036724754357,-0.91938970034031));
#8324=CARTESIAN_POINT('Ctrl Pts',(5.93158296354498,-1.81030185128305,-0.919379791771803));
#8325=CARTESIAN_POINT('Ctrl Pts',(5.93185451897547,-1.81017615747267,-0.919360750892484));
#8326=CARTESIAN_POINT('Ctrl Pts',(5.93198474668212,-1.81011586241321,-0.919351618666983));
#8327=CARTESIAN_POINT('Ctrl Pts',(5.93223499665919,-1.80999996458596,-0.919334068064972));
#8328=CARTESIAN_POINT('Ctrl Pts',(5.93235501992212,-1.8099443639256,-0.91932564976036));
#8329=CARTESIAN_POINT('Ctrl Pts',(5.93258568350518,-1.80983748137534,-0.919309469724261));
#8330=CARTESIAN_POINT('Ctrl Pts',(5.93269632465075,-1.80978620127925,-0.919301708054864));
#8331=CARTESIAN_POINT('Ctrl Pts',(5.93290897811127,-1.80968761669767,-0.919286788737124));
#8332=CARTESIAN_POINT('Ctrl Pts',(5.93301099113292,-1.80964031373031,-0.919279631140989));
#8333=CARTESIAN_POINT('Ctrl Pts',(5.93320707983826,-1.80954936815609,-0.919265871749315));
#8334=CARTESIAN_POINT('Ctrl Pts',(5.93330115611567,-1.80950572683993,-0.919259269998498));
#8335=CARTESIAN_POINT('Ctrl Pts',(5.93348200544767,-1.80942181498176,-0.919246578050966));
#8336=CARTESIAN_POINT('Ctrl Pts',(5.93356877901262,-1.80938154553232,-0.919240487891772));
#8337=CARTESIAN_POINT('Ctrl Pts',(5.93373560456005,-1.80930411136666,-0.919228778519481));
#8338=CARTESIAN_POINT('Ctrl Pts',(5.93381565697793,-1.80926694757728,-0.919223159338115));
#8339=CARTESIAN_POINT('Ctrl Pts',(5.93396957384581,-1.80919548030332,-0.919212354646954));
#8340=CARTESIAN_POINT('Ctrl Pts',(5.93404343867405,-1.80916117760223,-0.919207169163538));
#8341=CARTESIAN_POINT('Ctrl Pts',(5.9341854701528,-1.80909520784966,-0.919197197638442));
#8342=CARTESIAN_POINT('Ctrl Pts',(5.93425363709459,-1.80906354147808,-0.919192411621305));
#8343=CARTESIAN_POINT('Ctrl Pts',(5.93438472234664,-1.80900263793383,-0.919183207597438));
#8344=CARTESIAN_POINT('Ctrl Pts',(5.93444764093444,-1.80897340132536,-0.919178789609484));
#8345=CARTESIAN_POINT('Ctrl Pts',(5.93456864237285,-1.80891716747187,-0.919170292763325));
#8346=CARTESIAN_POINT('Ctrl Pts',(5.93462672545113,-1.80889017071065,-0.919166213921685));
#8347=CARTESIAN_POINT('Ctrl Pts',(5.93473843517084,-1.80883824197768,-0.919158368827159));
#8348=CARTESIAN_POINT('Ctrl Pts',(5.93479206200654,-1.80881331041736,-0.919154602588332));
#8349=CARTESIAN_POINT('Ctrl Pts',(5.93493162711471,-1.80874841789375,-0.919144800445906));
#8350=CARTESIAN_POINT('Ctrl Pts',(5.93501756365072,-1.80870845318935,-0.919138764413097));
#8351=CARTESIAN_POINT('Ctrl Pts',(5.93518796475567,-1.80862919354634,-0.919126794920098));
#8352=CARTESIAN_POINT('Ctrl Pts',(5.93527242941148,-1.80858989881938,-0.919120861467726));
#8353=CARTESIAN_POINT('Ctrl Pts',(5.94402968012073,-1.80451509611075,-0.918505643051591));
#8354=CARTESIAN_POINT('Ctrl Pts',(5.95267320169202,-1.80041732069438,-0.917894221385039));
#8355=CARTESIAN_POINT('Ctrl Pts',(5.97742726585404,-1.78846293752613,-0.916130905918012));
#8356=CARTESIAN_POINT('Ctrl Pts',(5.99346149258386,-1.78045130761798,-0.914973677976082));
#8357=CARTESIAN_POINT('Ctrl Pts',(6.02949121042656,-1.76183781424405,-0.912338332072786));
#8358=CARTESIAN_POINT('Ctrl Pts',(6.04941833475516,-1.75110968723624,-0.910855947989299));
#8359=CARTESIAN_POINT('Ctrl Pts',(6.11341436099436,-1.71523860952733,-0.906013006214644));
#8360=CARTESIAN_POINT('Ctrl Pts',(6.15670492268725,-1.68875448350377,-0.90260761709076));
#8361=CARTESIAN_POINT('Ctrl Pts',(6.29692086832602,-1.59544534311504,-0.891148584970972));
#8362=CARTESIAN_POINT('Ctrl Pts',(6.38893642939663,-1.52169912646323,-0.882899299916485));
#8363=CARTESIAN_POINT('Ctrl Pts',(6.53825559993723,-1.37862135605198,-0.868524620877928));
#8364=CARTESIAN_POINT('Ctrl Pts',(6.59840852010042,-1.31271055972378,-0.862391087466903));
#8365=CARTESIAN_POINT('Ctrl Pts',(6.66077822635619,-1.23442770256218,-0.855812460215527));
#8366=CARTESIAN_POINT('Ctrl Pts',(6.66752956696062,-1.22580917944168,-0.855097218842239));
#8367=CARTESIAN_POINT('Ctrl Pts',(6.67764605651602,-1.21267347903028,-0.854021243135279));
#8368=CARTESIAN_POINT('Ctrl Pts',(6.68106346401881,-1.20819707860783,-0.853657025913144));
#8369=CARTESIAN_POINT('Ctrl Pts',(6.68717551216369,-1.20012032677696,-0.853004362245831));
#8370=CARTESIAN_POINT('Ctrl Pts',(6.68987696438829,-1.19652529983947,-0.852715450252279));
#8371=CARTESIAN_POINT('Ctrl Pts',(6.6957856890142,-1.18860649458396,-0.852082556000752));
#8372=CARTESIAN_POINT('Ctrl Pts',(6.6989876211743,-1.18427886206775,-0.851738941007445));
#8373=CARTESIAN_POINT('Ctrl Pts',(6.70814701355804,-1.17179391908996,-0.850753952284036));
#8374=CARTESIAN_POINT('Ctrl Pts',(6.71406018725152,-1.16360411045334,-0.850115535109336));
#8375=CARTESIAN_POINT('Ctrl Pts',(6.75653348249325,-1.10382657714879,-0.845508573168104));
#8376=CARTESIAN_POINT('Ctrl Pts',(6.79068861253648,-1.05056573398017,-0.841687154181984));
#8377=CARTESIAN_POINT('Ctrl Pts',(6.89065319632637,-0.877049248422192,-0.829811551901653));
#8378=CARTESIAN_POINT('Ctrl Pts',(6.94663611327104,-0.751599042259346,-0.822029168856653));
#8379=CARTESIAN_POINT('Ctrl Pts',(7.00605985538138,-0.570334324611354,-0.810777203479737));
#8380=CARTESIAN_POINT('Ctrl Pts',(7.02072836573836,-0.518619563541358,-0.807569791955741));
#8381=CARTESIAN_POINT('Ctrl Pts',(7.04192617252939,-0.430467145676259,-0.802055639977398));
#8382=CARTESIAN_POINT('Ctrl Pts',(7.04956212402777,-0.394325005806245,-0.799782079915123));
#8383=CARTESIAN_POINT('Ctrl Pts',(7.05855933362424,-0.34500624662049,-0.79665284697295));
#8384=CARTESIAN_POINT('Ctrl Pts',(7.06079954751239,-0.331996141197615,-0.795824881290785));
#8385=CARTESIAN_POINT('Ctrl Pts',(7.06414771905988,-0.311326699292858,-0.794505148165942));
#8386=CARTESIAN_POINT('Ctrl Pts',(7.06534055155126,-0.303681351655337,-0.794016061946849));
#8387=CARTESIAN_POINT('Ctrl Pts',(7.06764215613092,-0.288344063952135,-0.793032950706052));
#8388=CARTESIAN_POINT('Ctrl Pts',(7.06875051989567,-0.280652200958789,-0.792538922112808));
#8389=CARTESIAN_POINT('Ctrl Pts',(7.07088754748584,-0.265181697031638,-0.791543236316246));
#8390=CARTESIAN_POINT('Ctrl Pts',(7.07191531843868,-0.257403074466527,-0.791041560441624));
#8391=CARTESIAN_POINT('Ctrl Pts',(7.07416351688411,-0.239578518695906,-0.789889517242021));
#8392=CARTESIAN_POINT('Ctrl Pts',(7.07535343413771,-0.229529021409757,-0.789238205857419));
#8393=CARTESIAN_POINT('Ctrl Pts',(7.07938889522422,-0.193073803378723,-0.786868827789353));
#8394=CARTESIAN_POINT('Ctrl Pts',(7.08178337595365,-0.16662193566441,-0.785136834312907));
#8395=CARTESIAN_POINT('Ctrl Pts',(7.08696839595962,-0.0929961565994294,
-0.780278748685038));
#8396=CARTESIAN_POINT('Ctrl Pts',(7.08861171172832,-0.0457620549677525,
-0.777119293896236));
#8397=CARTESIAN_POINT('Ctrl Pts',(7.08857660471327,0.00148228751319614,
-0.773917982071593));
#8398=CARTESIAN_POINT('Origin',(5.09382715545311,0.,-6.77268258743872));
#8399=CARTESIAN_POINT('',(7.08857715545311,-1.12589837781526E-10,0.186011338956535));
#8400=CARTESIAN_POINT('',(7.08880671729685,0.00054701437290982,0.0273173682685466));
#8401=CARTESIAN_POINT('',(7.08857715545311,8.3550772080578E-14,-6.77268258743872));
#8402=CARTESIAN_POINT('Ctrl Pts',(7.08857715545311,-1.12589837781526E-10,
0.186011338956534));
#8403=CARTESIAN_POINT('Ctrl Pts',(7.08857715545308,-0.000600192261292308,
0.185969784536992));
#8404=CARTESIAN_POINT('Ctrl Pts',(7.0885768845847,-0.00120038994982216,
0.185928226101576));
#8405=CARTESIAN_POINT('Ctrl Pts',(7.08846930102655,-0.120384617245889,0.177675041757695));
#8406=CARTESIAN_POINT('Ctrl Pts',(7.0777883325812,-0.238722073627921,0.169320437128287));
#8407=CARTESIAN_POINT('Ctrl Pts',(7.04839332461821,-0.401062440880801,0.158061675733446));
#8408=CARTESIAN_POINT('Ctrl Pts',(7.03853620070026,-0.446416258112179,0.154941279742027));
#8409=CARTESIAN_POINT('Ctrl Pts',(7.02492514575313,-0.499966444455275,0.15131812106603));
#8410=CARTESIAN_POINT('Ctrl Pts',(7.02268779462601,-0.50852977814502,0.15074062684239));
#8411=CARTESIAN_POINT('Ctrl Pts',(7.01893366416992,-0.52251718346597,0.149800763933142));
#8412=CARTESIAN_POINT('Ctrl Pts',(7.01745080661349,-0.527950118378297,0.149436553642766));
#8413=CARTESIAN_POINT('Ctrl Pts',(7.01474251373248,-0.537709931890585,0.148783897283026));
#8414=CARTESIAN_POINT('Ctrl Pts',(7.01352544364508,-0.542038991238084,0.14849498571365));
#8415=CARTESIAN_POINT('Ctrl Pts',(7.01081919459467,-0.551541535177392,0.147862086371448));
#8416=CARTESIAN_POINT('Ctrl Pts',(7.00932371039755,-0.556713115340731,0.147518465904997));
#8417=CARTESIAN_POINT('Ctrl Pts',(7.00496192756431,-0.571571066731513,0.146533445501946));
#8418=CARTESIAN_POINT('Ctrl Pts',(7.00204291482573,-0.581241969653556,0.145895002416735));
#8419=CARTESIAN_POINT('Ctrl Pts',(6.98031707328297,-0.651293153351429,0.141287253539343));
#8420=CARTESIAN_POINT('Ctrl Pts',(6.958719665787,-0.710777483463359,0.137465130731298));
#8421=CARTESIAN_POINT('Ctrl Pts',(6.88373666759687,-0.890206795267031,0.12593270731537));
#8422=CARTESIAN_POINT('Ctrl Pts',(6.82132079467698,-1.00598840618957,0.1184670754301));
#8423=CARTESIAN_POINT('Ctrl Pts',(6.69848112489066,-1.18825888437743,0.105534450798882));
#8424=CARTESIAN_POINT('Ctrl Pts',(6.64414608460326,-1.2583250367509,0.100226027108668));
#8425=CARTESIAN_POINT('Ctrl Pts',(6.57495118299308,-1.33624247705346,0.0937587316688997));
#8426=CARTESIAN_POINT('Ctrl Pts',(6.56442533891264,-1.3478179786439,0.0927823067676446));
#8427=CARTESIAN_POINT('Ctrl Pts',(6.54691963810087,-1.36662017578259,0.0911696172275229));
#8428=CARTESIAN_POINT('Ctrl Pts',(6.5400192941925,-1.37392021599271,0.090536714667003));
#8429=CARTESIAN_POINT('Ctrl Pts',(6.5274988892059,-1.38696702449002,0.0893931256753902));
#8430=CARTESIAN_POINT('Ctrl Pts',(6.52189863819049,-1.39273256740069,0.0888832996976042));
#8431=CARTESIAN_POINT('Ctrl Pts',(6.50986696334501,-1.40497049004328,0.0877914700335683));
#8432=CARTESIAN_POINT('Ctrl Pts',(6.50342568827995,-1.41143288438844,0.0872090410970939));
#8433=CARTESIAN_POINT('Ctrl Pts',(6.48584351007915,-1.42883230850661,0.0856247152244667));
#8434=CARTESIAN_POINT('Ctrl Pts',(6.47461836137105,-1.43968292347054,0.084619091990734));
#8435=CARTESIAN_POINT('Ctrl Pts',(6.41403111114575,-1.49688823714525,0.0792210716612793));
#8436=CARTESIAN_POINT('Ctrl Pts',(6.36246518406953,-1.54083375273024,0.0747283949014611));
#8437=CARTESIAN_POINT('Ctrl Pts',(6.17799610270443,-1.68249594039927,0.0589868787249901));
#8438=CARTESIAN_POINT('Ctrl Pts',(6.03529593146887,-1.76630720326369,0.0472957275249053));
#8439=CARTESIAN_POINT('Ctrl Pts',(5.83481567995111,-1.85278816885954,0.0323285036762399));
#8440=CARTESIAN_POINT('Ctrl Pts',(5.78486989871763,-1.87199065581956,0.0287159183836105));
#8441=CARTESIAN_POINT('Ctrl Pts',(5.72548284609896,-1.89212143641683,0.0246008843656744));
#8442=CARTESIAN_POINT('Ctrl Pts',(5.71673693296706,-1.89501869608009,0.0239993795893232));
#8443=CARTESIAN_POINT('Ctrl Pts',(5.70250871307328,-1.89962293248718,0.0230284919898422));
#8444=CARTESIAN_POINT('Ctrl Pts',(5.69703867436649,-1.9013669792164,0.0226570640384776));
#8445=CARTESIAN_POINT('Ctrl Pts',(5.68726471019914,-1.90443684879979,0.0219967456655443));
#8446=CARTESIAN_POINT('Ctrl Pts',(5.68296375886098,-1.90577173509957,0.021707339220391));
#8447=CARTESIAN_POINT('Ctrl Pts',(5.67359479394345,-1.9086448325516,0.0210794467096769));
#8448=CARTESIAN_POINT('Ctrl Pts',(5.66852516676361,-1.9101774286243,0.0207412862329052));
#8449=CARTESIAN_POINT('Ctrl Pts',(5.65416079596607,-1.91445755050441,0.0197874939278794));
#8450=CARTESIAN_POINT('Ctrl Pts',(5.64485189624997,-1.91715759534056,0.019174534532152));
#8451=CARTESIAN_POINT('Ctrl Pts',(5.58457425549715,-1.93416579929945,0.0152364533001346));
#8452=CARTESIAN_POINT('Ctrl Pts',(5.53306792423637,-1.94650935721105,0.0120140479844558));
#8453=CARTESIAN_POINT('Ctrl Pts',(5.31603016415036,-1.98946678000028,-0.00120430811957895));
#8454=CARTESIAN_POINT('Ctrl Pts',(5.14745808018485,-2.00112036177713,-0.0106641100520869));
#8455=CARTESIAN_POINT('Ctrl Pts',(4.91461712540124,-1.98774345746366,-0.0245610189936562));
#8456=CARTESIAN_POINT('Ctrl Pts',(4.85004457780563,-1.98086068640027,-0.0284964312311433));
#8457=CARTESIAN_POINT('Ctrl Pts',(4.77024309358754,-1.96839348115497,-0.0335175945513442));
#8458=CARTESIAN_POINT('Ctrl Pts',(4.75458965566949,-1.965756199963,-0.034510044728272));
#8459=CARTESIAN_POINT('Ctrl Pts',(4.72984386099876,-1.96128267382114,-0.0360916198212695));
#8460=CARTESIAN_POINT('Ctrl Pts',(4.72072975818503,-1.95956931307585,-0.0366768596795332));
#8461=CARTESIAN_POINT('Ctrl Pts',(4.70375395364451,-1.95625530648223,-0.0377721625827098));
#8462=CARTESIAN_POINT('Ctrl Pts',(4.69588929178882,-1.95467065780994,-0.0382817083412731));
#8463=CARTESIAN_POINT('Ctrl Pts',(4.67840161737721,-1.95103715573355,-0.0394195147352495));
#8464=CARTESIAN_POINT('Ctrl Pts',(4.66878382354482,-1.9489644740296,-0.0400485224361274));
#8465=CARTESIAN_POINT('Ctrl Pts',(4.64066423237808,-1.94268652217119,-0.0418972659175536));
#8466=CARTESIAN_POINT('Ctrl Pts',(4.62220704824959,-1.93828841807665,-0.0431231107221309));
#8467=CARTESIAN_POINT('Ctrl Pts',(4.48263948960501,-1.90291983745407,-0.0524894446724259));
#8468=CARTESIAN_POINT('Ctrl Pts',(4.36463966305213,-1.86089488315989,-0.0609911000013024));
#8469=CARTESIAN_POINT('Ctrl Pts',(4.12747487632397,-1.75039191044516,-0.079152725547265));
#8470=CARTESIAN_POINT('Ctrl Pts',(4.00984097859791,-1.68008511467575,-0.0887996469414836));
#8471=CARTESIAN_POINT('Ctrl Pts',(3.88182034174079,-1.58448727905861,-0.0994816523230889));
#8472=CARTESIAN_POINT('Ctrl Pts',(3.86356404598011,-1.57035449673139,-0.101008952652158));
#8473=CARTESIAN_POINT('Ctrl Pts',(3.83952866578315,-1.55107142936336,-0.103020665602361));
#8474=CARTESIAN_POINT('Ctrl Pts',(3.83352906705225,-1.5462005087499,-0.103522898672078));
#8475=CARTESIAN_POINT('Ctrl Pts',(3.82417310226454,-1.53851400270541,-0.104306018192094));
#8476=CARTESIAN_POINT('Ctrl Pts',(3.82079752426466,-1.53572208107877,-0.104588546945842));
#8477=CARTESIAN_POINT('Ctrl Pts',(3.81392477006144,-1.52999943300144,-0.10516370018827));
#8478=CARTESIAN_POINT('Ctrl Pts',(3.81042844376182,-1.52706782046322,-0.105456241705951));
#8479=CARTESIAN_POINT('Ctrl Pts',(3.80217776756194,-1.52010141229719,-0.106146527497702));
#8480=CARTESIAN_POINT('Ctrl Pts',(3.79743217725701,-1.51605623507771,-0.106543522255797));
#8481=CARTESIAN_POINT('Ctrl Pts',(3.78168205223525,-1.50250267717501,-0.107861274034392));
#8482=CARTESIAN_POINT('Ctrl Pts',(3.77076224015238,-1.49289595271181,-0.108775166391714));
#8483=CARTESIAN_POINT('Ctrl Pts',(3.71001425204032,-1.43826266685922,-0.11386729567284));
#8484=CARTESIAN_POINT('Ctrl Pts',(3.66237473750464,-1.39085710770181,-0.117892114403733));
#8485=CARTESIAN_POINT('Ctrl Pts',(3.50442823448687,-1.21695500812358,-0.13173793511042));
#8486=CARTESIAN_POINT('Ctrl Pts',(3.40776079220736,-1.07905057996273,-0.141215259364283));
#8487=CARTESIAN_POINT('Ctrl Pts',(3.3076738741116,-0.889309216331047,-0.154158667736021));
#8488=CARTESIAN_POINT('Ctrl Pts',(3.28731837813025,-0.847195339820908,-0.15702113546422));
#8489=CARTESIAN_POINT('Ctrl Pts',(3.26264628460628,-0.791209327991986,-0.160833108224414));
#8490=CARTESIAN_POINT('Ctrl Pts',(3.25697351173675,-0.777948749480136,-0.161736423544074));
#8491=CARTESIAN_POINT('Ctrl Pts',(3.24804760690145,-0.756441657777049,-0.163202714999555));
#8492=CARTESIAN_POINT('Ctrl Pts',(3.24470470826121,-0.748232781071678,-0.163762655686476));
#8493=CARTESIAN_POINT('Ctrl Pts',(3.23841614017006,-0.732490919022245,-0.164837098741973));
#8494=CARTESIAN_POINT('Ctrl Pts',(3.23546135586276,-0.724961746472034,-0.165351282759005));
#8495=CARTESIAN_POINT('Ctrl Pts',(3.22877622929245,-0.70761772870826,-0.166536507299769));
#8496=CARTESIAN_POINT('Ctrl Pts',(3.22507745338121,-0.697791051256904,-0.167208583873025));
#8497=CARTESIAN_POINT('Ctrl Pts',(3.21375240750098,-0.666967412995959,-0.169318703382814));
#8498=CARTESIAN_POINT('Ctrl Pts',(3.20640137475594,-0.645871847374074,-0.170765763156876));
#8499=CARTESIAN_POINT('Ctrl Pts',(3.17178107201273,-0.540877717004986,-0.17798482425887));
#8500=CARTESIAN_POINT('Ctrl Pts',(3.14974749998642,-0.455368485299618,-0.183923610536241));
#8501=CARTESIAN_POINT('Ctrl Pts',(3.11346522651393,-0.262450980989509,-0.197411632423579));
#8502=CARTESIAN_POINT('Ctrl Pts',(3.10215444585066,-0.15476398699513,-0.205004033418503));
#8503=CARTESIAN_POINT('Ctrl Pts',(3.09781469267797,0.0305591832669149,-0.217847915183087));
#8504=CARTESIAN_POINT('Ctrl Pts',(3.1004964726237,0.107866218868336,-0.223135399237172));
#8505=CARTESIAN_POINT('Ctrl Pts',(3.10866033654096,0.195594300054974,-0.228924947609783));
#8506=CARTESIAN_POINT('Ctrl Pts',(3.10974953183513,0.206350248483781,-0.229631102878834));
#8507=CARTESIAN_POINT('Ctrl Pts',(3.11153585827572,0.222666028907593,-0.230696156430305));
#8508=CARTESIAN_POINT('Ctrl Pts',(3.11216903756611,0.228232453777321,-0.231058435535144));
#8509=CARTESIAN_POINT('Ctrl Pts',(3.11335259633733,0.238260980750037,-0.231709078251876));
#8510=CARTESIAN_POINT('Ctrl Pts',(3.11389461380411,0.242723929417162,-0.231997893765927));
#8511=CARTESIAN_POINT('Ctrl Pts',(3.11512197098991,0.252552192257652,-0.232632296430501));
#8512=CARTESIAN_POINT('Ctrl Pts',(3.11581404464018,0.257916560050992,-0.232977504315233));
#8513=CARTESIAN_POINT('Ctrl Pts',(3.11787704316272,0.273410309871004,-0.233971678132952));
#8514=CARTESIAN_POINT('Ctrl Pts',(3.11930404141261,0.283532231647796,-0.234617601285223));
#8515=CARTESIAN_POINT('Ctrl Pts',(3.13066109229315,0.359841459175427,-0.239463345375374));
#8516=CARTESIAN_POINT('Ctrl Pts',(3.14383990919655,0.425509820343862,-0.24349815008954));
#8517=CARTESIAN_POINT('Ctrl Pts',(3.19691375458047,0.634768200016442,-0.256270576132744));
#8518=CARTESIAN_POINT('Ctrl Pts',(3.24958366131185,0.774583600701349,-0.264706931228053));
#8519=CARTESIAN_POINT('Ctrl Pts',(3.34862979051256,0.968529986462011,-0.277652424679086));
#8520=CARTESIAN_POINT('Ctrl Pts',(3.38307949114601,1.02815616797849,-0.28181718267952));
#8521=CARTESIAN_POINT('Ctrl Pts',(3.4293263517402,1.09942040651705,-0.287096665412004));
#8522=CARTESIAN_POINT('Ctrl Pts',(3.43827788540632,1.11285432394628,-0.288105668525936));
#8523=CARTESIAN_POINT('Ctrl Pts',(3.45266161187775,1.13388287109671,-0.289707757397677));
#8524=CARTESIAN_POINT('Ctrl Pts',(3.45798589262008,1.14155072810215,-0.290296784141614));
#8525=CARTESIAN_POINT('Ctrl Pts',(3.46798341343878,1.15573525997183,-0.291395593532152));
#8526=CARTESIAN_POINT('Ctrl Pts',(3.47264252424855,1.16226169732652,-0.291904830710072));
#8527=CARTESIAN_POINT('Ctrl Pts',(3.48306080503986,1.17667099585416,-0.293037399693551));
#8528=CARTESIAN_POINT('Ctrl Pts',(3.48883871927485,1.1845399876176,-0.293661445191679));
#8529=CARTESIAN_POINT('Ctrl Pts',(3.50579451151298,1.20728040810507,-0.295481250446377));
#8530=CARTESIAN_POINT('Ctrl Pts',(3.51712271804736,1.22203794553453,-0.296682831735835));
#8531=CARTESIAN_POINT('Ctrl Pts',(3.6204989940738,1.35287824933403,-0.307525801938078));
#8532=CARTESIAN_POINT('Ctrl Pts',(3.724988658736,1.45850619327345,-0.3176892073628));
#8533=CARTESIAN_POINT('Ctrl Pts',(3.93639982503237,1.6293225136517,-0.33662610749281));
#8534=CARTESIAN_POINT('Ctrl Pts',(4.039650773892,1.69795386080959,-0.34529703567476));
#8535=CARTESIAN_POINT('Ctrl Pts',(4.16259178078155,1.76410901412941,-0.354546599378821));
#8536=CARTESIAN_POINT('Ctrl Pts',(4.17667124427512,1.77146973137946,-0.355590703907002));
#8537=CARTESIAN_POINT('Ctrl Pts',(4.19618130207751,1.78137458119246,-0.357015238490354));
#8538=CARTESIAN_POINT('Ctrl Pts',(4.20153722570376,1.78406338454955,-0.357404014117713));
#8539=CARTESIAN_POINT('Ctrl Pts',(4.2107332661,1.78862824796189,-0.358067519356253));
#8540=CARTESIAN_POINT('Ctrl Pts',(4.21456740515156,1.79051615998201,-0.358342967401517));
#8541=CARTESIAN_POINT('Ctrl Pts',(4.22256765028322,1.79442354842247,-0.358915191732509));
#8542=CARTESIAN_POINT('Ctrl Pts',(4.22673475147267,1.79644085901353,-0.359211823722823));
#8543=CARTESIAN_POINT('Ctrl Pts',(4.23687644678574,1.80130698550387,-0.359930384937204));
#8544=CARTESIAN_POINT('Ctrl Pts',(4.24285833945941,1.80414064038547,-0.360351388247232));
#8545=CARTESIAN_POINT('Ctrl Pts',(4.26415070771659,1.81409748879608,-0.361840309495893));
#8546=CARTESIAN_POINT('Ctrl Pts',(4.27953789704593,1.8210562195592,-0.362898694307669));
#8547=CARTESIAN_POINT('Ctrl Pts',(4.31787080086471,1.83780891640602,-0.365496494217798));
#8548=CARTESIAN_POINT('Ctrl Pts',(4.34091587791336,1.84736964397415,-0.3670242046751));
#8549=CARTESIAN_POINT('Ctrl Pts',(4.43877987365078,1.88583488331559,-0.373393810163138));
#8550=CARTESIAN_POINT('Ctrl Pts',(4.51513196957062,1.91064753556587,-0.378078054703925));
#8551=CARTESIAN_POINT('Ctrl Pts',(4.74474081461945,1.9702321680669,-0.391866676259247));
#8552=CARTESIAN_POINT('Ctrl Pts',(4.90081118493827,1.99158602882379,-0.400906347312344));
#8553=CARTESIAN_POINT('Ctrl Pts',(5.08197402114595,1.99486173466594,-0.412065013907606));
#8554=CARTESIAN_POINT('Ctrl Pts',(5.10618827807214,1.99485863187619,-0.413568766245585));
#8555=CARTESIAN_POINT('Ctrl Pts',(5.1411195981775,1.99421814958416,-0.415758332265714));
#8556=CARTESIAN_POINT('Ctrl Pts',(5.15184156994278,1.99393503500094,-0.416433157918545));
#8557=CARTESIAN_POINT('Ctrl Pts',(5.17070500818579,1.9932846683157,-0.417625457157231));
#8558=CARTESIAN_POINT('Ctrl Pts',(5.17884754672173,1.99295396410719,-0.418141782162685));
#8559=CARTESIAN_POINT('Ctrl Pts',(5.19566232732439,1.99216780752531,-0.419211550951107));
#8560=CARTESIAN_POINT('Ctrl Pts',(5.20433406563859,1.99170559934392,-0.419765194565772));
#8561=CARTESIAN_POINT('Ctrl Pts',(5.22658096692162,1.9903740919839,-0.421190652674178));
#8562=CARTESIAN_POINT('Ctrl Pts',(5.24015058068346,1.9894225394784,-0.422065011721406));
#8563=CARTESIAN_POINT('Ctrl Pts',(5.29756005070113,1.9848062389891,-0.425785593836174));
#8564=CARTESIAN_POINT('Ctrl Pts',(5.34127920689039,1.97983077014022,-0.428672223842259));
#8565=CARTESIAN_POINT('Ctrl Pts',(5.54159408987943,1.95029552357698,-0.44215361767715));
#8566=CARTESIAN_POINT('Ctrl Pts',(5.69506043980011,1.90857317245293,-0.45326750700625));
#8567=CARTESIAN_POINT('Ctrl Pts',(5.92177897452171,1.81684907451172,-0.470255489441496));
#8568=CARTESIAN_POINT('Ctrl Pts',(5.9994501193327,1.77940868906003,-0.476173968018696));
#8569=CARTESIAN_POINT('Ctrl Pts',(6.08396940890362,1.73169425757625,-0.482552846946853));
#8570=CARTESIAN_POINT('Ctrl Pts',(6.09342978908017,1.72625063981266,-0.483265881719269));
#8571=CARTESIAN_POINT('Ctrl Pts',(6.10769714252797,1.71788441028284,-0.484339206088336));
#8572=CARTESIAN_POINT('Ctrl Pts',(6.1125370389865,1.71501876749111,-0.48470295366314));
#8573=CARTESIAN_POINT('Ctrl Pts',(6.12115311422296,1.70986795307525,-0.485349779423056));
#8574=CARTESIAN_POINT('Ctrl Pts',(6.12493387149097,1.70759069562882,-0.485633351656116));
#8575=CARTESIAN_POINT('Ctrl Pts',(6.13318026817938,1.70258628182991,-0.4862512995475));
#8576=CARTESIAN_POINT('Ctrl Pts',(6.1376427408819,1.69985410113087,-0.48658534388251));
#8577=CARTESIAN_POINT('Ctrl Pts',(6.14692190644068,1.69412254670215,-0.487279322380664));
#8578=CARTESIAN_POINT('Ctrl Pts',(6.15173666423004,1.69112011130864,-0.487639058884533));
#8579=CARTESIAN_POINT('Ctrl Pts',(6.16410249493643,1.68333542300669,-0.488562240127163));
#8580=CARTESIAN_POINT('Ctrl Pts',(6.1716344459629,1.67852283269386,-0.48912383253046));
#8581=CARTESIAN_POINT('Ctrl Pts',(6.19369522189635,1.66421723021552,-0.490767401613386));
#8582=CARTESIAN_POINT('Ctrl Pts',(6.20813316916562,1.65458481313967,-0.491841368111471));
#8583=CARTESIAN_POINT('Ctrl Pts',(6.25964969823477,1.61923482003678,-0.495674339848237));
#8584=CARTESIAN_POINT('Ctrl Pts',(6.29598087199812,1.59244798352437,-0.498379345324519));
#8585=CARTESIAN_POINT('Ctrl Pts',(6.44726128406627,1.47277868799808,-0.50979376172227));
#8586=CARTESIAN_POINT('Ctrl Pts',(6.55260429089217,1.36851489123446,-0.518165350263008));
#8587=CARTESIAN_POINT('Ctrl Pts',(6.68957658443352,1.1989735512608,-0.531111383008197));
#8588=CARTESIAN_POINT('Ctrl Pts',(6.73076826020462,1.1420928403117,-0.53535578063878));
#8589=CARTESIAN_POINT('Ctrl Pts',(6.77769092777207,1.06952979588961,-0.540725176889794));
#8590=CARTESIAN_POINT('Ctrl Pts',(6.78634048741768,1.05578870271875,-0.54173994028905));
#8591=CARTESIAN_POINT('Ctrl Pts',(6.79970839947311,1.03396532154878,-0.543349165718451));
#8592=CARTESIAN_POINT('Ctrl Pts',(6.80453939015688,1.02595260616638,-0.54393950741807));
#8593=CARTESIAN_POINT('Ctrl Pts',(6.81336600280249,1.01107703689446,-0.545034690982643));
#8594=CARTESIAN_POINT('Ctrl Pts',(6.81737737476225,1.00422371044698,-0.545538949189676));
#8595=CARTESIAN_POINT('Ctrl Pts',(6.82619894064773,0.988943731945201,-0.546662649974919));
#8596=CARTESIAN_POINT('Ctrl Pts',(6.83098876288862,0.980505610014253,-0.547282808412147));
#8597=CARTESIAN_POINT('Ctrl Pts',(6.84464223173192,0.956038502928189,-0.54908009376178));
#8598=CARTESIAN_POINT('Ctrl Pts',(6.85334672117221,0.93992229001771,-0.550262823121048));
#8599=CARTESIAN_POINT('Ctrl Pts',(6.92753536883622,0.797920395550181,-0.560677162917791));
#8600=CARTESIAN_POINT('Ctrl Pts',(6.9796230408858,0.665523982844454,-0.570384737091377));
#8601=CARTESIAN_POINT('Ctrl Pts',(7.04888150915202,0.413587693016349,-0.58857494240901));
#8602=CARTESIAN_POINT('Ctrl Pts',(7.07013529736856,0.295807504302604,-0.596960125366271));
#8603=CARTESIAN_POINT('Ctrl Pts',(7.08287314345197,0.152680432198282,-0.606579315606909));
#8604=CARTESIAN_POINT('Ctrl Pts',(7.08458189315883,0.128494970074411,-0.608184763692582));
#8605=CARTESIAN_POINT('Ctrl Pts',(7.08626098919135,0.0964207779197302,-0.610282291731446));
#8606=CARTESIAN_POINT('Ctrl Pts',(7.08662604221146,0.0885559153652952,-0.610794110692069));
#8607=CARTESIAN_POINT('Ctrl Pts',(7.08714258508254,0.0757966629662215,-0.611620144125036));
#8608=CARTESIAN_POINT('Ctrl Pts',(7.08732263219669,0.070903607618745,-0.611935896173381));
#8609=CARTESIAN_POINT('Ctrl Pts',(7.08762640562701,0.0617289170494633,-0.612525962807788));
#8610=CARTESIAN_POINT('Ctrl Pts',(7.08775435910392,0.0574475070171664,-0.612800505435861));
#8611=CARTESIAN_POINT('Ctrl Pts',(7.08798983537845,0.0486156934111297,-0.613365214198298));
#8612=CARTESIAN_POINT('Ctrl Pts',(7.08809557641243,0.0440652447741042,-0.613655282533092));
#8613=CARTESIAN_POINT('Ctrl Pts',(7.08831313837811,0.0330845301316651,-0.614353189587575));
#8614=CARTESIAN_POINT('Ctrl Pts',(7.08840944037348,0.0266539590409399,-0.61476019777572));
#8615=CARTESIAN_POINT('Ctrl Pts',(7.08854128019806,0.013650208383668,-0.615579999299495));
#8616=CARTESIAN_POINT('Ctrl Pts',(7.08857543143116,0.00707710677119785,
-0.615992716324821));
#8617=CARTESIAN_POINT('Ctrl Pts',(7.08857709181507,0.000503868992114988,
-0.616403874612628));
#8618=CARTESIAN_POINT('Ctrl Pts',(7.08857666516212,0.0013985762946109,-0.772682587389958));
#8619=CARTESIAN_POINT('Ctrl Pts',(7.08852067831295,0.0812510236518176,-0.767603483263897));
#8620=CARTESIAN_POINT('Ctrl Pts',(7.08366576807236,0.160913471443935,-0.762524379137835));
#8621=CARTESIAN_POINT('Ctrl Pts',(7.07410411760675,0.239855614200625,-0.757445275011775));
#8622=CARTESIAN_POINT('Ctrl Pts',(7.06445696132819,0.319503703291223,-0.752320750596727));
#8623=CARTESIAN_POINT('Ctrl Pts',(7.05001861828069,0.398418352407743,-0.747196226181679));
#8624=CARTESIAN_POINT('Ctrl Pts',(7.0309335007,0.476074122069483,-0.742071701766631));
#8625=CARTESIAN_POINT('Ctrl Pts',(7.01328532357908,0.547883099491694,-0.737333008690473));
#8626=CARTESIAN_POINT('Ctrl Pts',(6.99166436661312,0.618615733605399,-0.732594315614317));
#8627=CARTESIAN_POINT('Ctrl Pts',(6.96622088098845,0.687873025402144,-0.72785562253816));
#8628=CARTESIAN_POINT('Ctrl Pts',(6.94229794684064,0.752991368672771,-0.723400122844453));
#8629=CARTESIAN_POINT('Ctrl Pts',(6.91492693121006,0.816988152165582,-0.718944623150746));
#8630=CARTESIAN_POINT('Ctrl Pts',(6.88423339278693,0.879473176291434,-0.71448912345704));
#8631=CARTESIAN_POINT('Ctrl Pts',(6.85358575018637,0.941864767019658,-0.7100402860393));
#8632=CARTESIAN_POINT('Ctrl Pts',(6.81962565955996,1.00274864955535,-0.705591448621559));
#8633=CARTESIAN_POINT('Ctrl Pts',(6.78252741640302,1.06175279192838,-0.701142611203819));
#8634=CARTESIAN_POINT('Ctrl Pts',(6.74547259460109,1.12068787335419,-0.696698980893814));
#8635=CARTESIAN_POINT('Ctrl Pts',(6.70528717467093,1.17774717229729,-0.692255350583809));
#8636=CARTESIAN_POINT('Ctrl Pts',(6.66219137591145,1.23258315520135,-0.687811720273803));
#8637=CARTESIAN_POINT('Ctrl Pts',(6.61912252451289,1.28738484972775,-0.683370868520251));
#8638=CARTESIAN_POINT('Ctrl Pts',(6.57314720612321,1.33996560245424,-0.6789300167667));
#8639=CARTESIAN_POINT('Ctrl Pts',(6.52452809064639,1.39000805628495,-0.674489165013148));
#8640=CARTESIAN_POINT('Ctrl Pts',(6.47592288711615,1.44003619089291,-0.670049583971574));
#8641=CARTESIAN_POINT('Ctrl Pts',(6.42467572905522,1.48752711785398,-0.665610002930001));
#8642=CARTESIAN_POINT('Ctrl Pts',(6.37108738870107,1.53219902723614,-0.661170421888427));
#8643=CARTESIAN_POINT('Ctrl Pts',(6.31749620837785,1.57687330405195,-0.656730605566701));
#8644=CARTESIAN_POINT('Ctrl Pts',(6.26156397672323,1.61872795532988,-0.652290789244975));
#8645=CARTESIAN_POINT('Ctrl Pts',(6.20362452957619,1.65752144809336,-0.64785097292325));
#8646=CARTESIAN_POINT('Ctrl Pts',(6.14562392296001,1.69635589032289,-0.643406470039558));
#8647=CARTESIAN_POINT('Ctrl Pts',(6.08561227932795,1.73212245212697,-0.638961967155866));
#8648=CARTESIAN_POINT('Ctrl Pts',(6.02395159099266,1.76462350004533,-0.634517464272174));
#8649=CARTESIAN_POINT('Ctrl Pts',(5.96225473111489,1.79714361380722,-0.630070354143426));
#8650=CARTESIAN_POINT('Ctrl Pts',(5.89890734530683,1.82639419570988,-0.625623244014679));
#8651=CARTESIAN_POINT('Ctrl Pts',(5.8342926167455,1.85222527332208,-0.621176133885931));
#8652=CARTESIAN_POINT('Ctrl Pts',(5.76956633062213,1.87810094838299,-0.616721345805497));
#8653=CARTESIAN_POINT('Ctrl Pts',(5.70356879718913,1.90054517729538,-0.612266557725061));
#8654=CARTESIAN_POINT('Ctrl Pts',(5.63669881869021,1.91945771502114,-0.607811769644627));
#8655=CARTESIAN_POINT('Ctrl Pts',(5.60275727216669,1.9290572512182,-0.605550629439731));
#8656=CARTESIAN_POINT('Ctrl Pts',(5.56859112792846,1.93774772530178,-0.603289489234835));
#8657=CARTESIAN_POINT('Ctrl Pts',(5.5342532709229,1.94552111253314,-0.601028349029939));
#8658=CARTESIAN_POINT('Ctrl Pts',(5.46659169423707,1.96083830708545,-0.596572849336225));
#8659=CARTESIAN_POINT('Ctrl Pts',(5.39799719595367,1.97265167236967,-0.592117349642511));
#8660=CARTESIAN_POINT('Ctrl Pts',(5.32886554407487,1.98085449197413,-0.587661849948798));
#8661=CARTESIAN_POINT('Ctrl Pts',(5.25983726424732,1.98904504596269,-0.583213012531049));
#8662=CARTESIAN_POINT('Ctrl Pts',(5.19027390689186,1.99363571273677,-0.5787641751133));
#8663=CARTESIAN_POINT('Ctrl Pts',(5.12058248328074,1.99457055902589,-0.574315337695551));
#8664=CARTESIAN_POINT('Ctrl Pts',(5.0509726294635,1.99550431113131,-0.56987170738554));
#8665=CARTESIAN_POINT('Ctrl Pts',(4.98123549391188,1.99279073491001,-0.565428077075528));
#8666=CARTESIAN_POINT('Ctrl Pts',(4.91178248827855,1.98642576041827,-0.560984446765517));
#8667=CARTESIAN_POINT('Ctrl Pts',(4.84237291089729,1.9800647658798,-0.556543595011961));
#8668=CARTESIAN_POINT('Ctrl Pts',(4.77324759700005,1.9700569470899,-0.552102743258405));
#8669=CARTESIAN_POINT('Ctrl Pts',(4.70481570474851,1.95645026865512,-0.54766189150485));
#8670=CARTESIAN_POINT('Ctrl Pts',(4.63640339370116,1.9428474836557,-0.54322231046327));
#8671=CARTESIAN_POINT('Ctrl Pts',(4.56868458993034,1.92564797875571,-0.538782729421691));
#8672=CARTESIAN_POINT('Ctrl Pts',(4.50205932653326,1.90495102277079,-0.534343148380112));
#8673=CARTESIAN_POINT('Ctrl Pts',(4.43543053226201,1.88425296992947,-0.529903332058381));
#8674=CARTESIAN_POINT('Ctrl Pts',(4.36989585984738,1.86005724545217,-0.52546351573665));
#8675=CARTESIAN_POINT('Ctrl Pts',(4.30583950838136,1.83251276409261,-0.521023699414919));
#8676=CARTESIAN_POINT('Ctrl Pts',(4.24171554059099,1.80493920744944,-0.516579196531222));
#8677=CARTESIAN_POINT('Ctrl Pts',(4.17907345852527,1.77401003240079,-0.512134693647524));
#8678=CARTESIAN_POINT('Ctrl Pts',(4.11827591922954,1.7399216499609,-0.507690190763827));
#8679=CARTESIAN_POINT('Ctrl Pts',(4.0574427147339,1.70581327051146,-0.503243080635074));
#8680=CARTESIAN_POINT('Ctrl Pts',(3.99845662035562,1.66854225629977,-0.49879597050632));
#8681=CARTESIAN_POINT('Ctrl Pts',(3.94165180747088,1.62834871265402,-0.494348860377566));
#8682=CARTESIAN_POINT('Ctrl Pts',(3.88474892087168,1.58808577471012,-0.489894072297126));
#8683=CARTESIAN_POINT('Ctrl Pts',(3.83003521680561,1.54489053865226,-0.485439284216686));
#8684=CARTESIAN_POINT('Ctrl Pts',(3.77781161784099,1.49904325063137,-0.480984496136245));
#8685=CARTESIAN_POINT('Ctrl Pts',(3.75130421117469,1.4757723016311,-0.478723355931404));
#8686=CARTESIAN_POINT('Ctrl Pts',(3.72543774509184,1.45181868636682,-0.476462215726563));
#8687=CARTESIAN_POINT('Ctrl Pts',(3.70024770244909,1.42722243209145,-0.474201075521722));
#8688=CARTESIAN_POINT('Ctrl Pts',(3.65061158212398,1.37875635150263,-0.469745575828008));
#8689=CARTESIAN_POINT('Ctrl Pts',(3.60340930693106,1.32760260275726,-0.465290076134292));
#8690=CARTESIAN_POINT('Ctrl Pts',(3.5589455818756,1.27403536748092,-0.460834576440577));
#8691=CARTESIAN_POINT('Ctrl Pts',(3.51454834310164,1.22054823089803,-0.456385739022829));
#8692=CARTESIAN_POINT('Ctrl Pts',(3.4728818367189,1.16465514408179,-0.451936901605084));
#8693=CARTESIAN_POINT('Ctrl Pts',(3.43421425417683,1.10666733050964,-0.447488064187336));
#8694=CARTESIAN_POINT('Ctrl Pts',(3.39559192981105,1.04874738833044,-0.443044433877322));
#8695=CARTESIAN_POINT('Ctrl Pts',(3.35996182778489,0.988737994062009,-0.438600803567306));
#8696=CARTESIAN_POINT('Ctrl Pts',(3.32755099966797,0.926982256574998,-0.434157173257293));
#8697=CARTESIAN_POINT('Ctrl Pts',(3.29516043770945,0.86526513431723,-0.429716321503735));
#8698=CARTESIAN_POINT('Ctrl Pts',(3.26598538302946,0.801804267298664,-0.425275469750176));
#8699=CARTESIAN_POINT('Ctrl Pts',(3.24020798668413,0.736969157883973,-0.420834617996618));
#8700=CARTESIAN_POINT('Ctrl Pts',(3.21443796632163,0.672152600484658,-0.416395036955037));
#8701=CARTESIAN_POINT('Ctrl Pts',(3.19206385483186,0.605963035687771,-0.411955455913459));
#8702=CARTESIAN_POINT('Ctrl Pts',(3.17321978051959,0.538790194649985,-0.407515874871877));
#8703=CARTESIAN_POINT('Ctrl Pts',(3.15437470754627,0.471613793718569,-0.403076058550144));
#8704=CARTESIAN_POINT('Ctrl Pts',(3.13906017295436,0.403454484730628,-0.398636242228407));
#8705=CARTESIAN_POINT('Ctrl Pts',(3.12736002732783,0.334715695034933,-0.394196425906673));
#8706=CARTESIAN_POINT('Ctrl Pts',(3.11564753131257,0.26590434634716,-0.389751923022975));
#8707=CARTESIAN_POINT('Ctrl Pts',(3.10755712127305,0.196512779279445,-0.385307420139277));
#8708=CARTESIAN_POINT('Ctrl Pts',(3.10312107163794,0.126952157765381,-0.380862917255578));
#8709=CARTESIAN_POINT('Ctrl Pts',(3.09868241971665,0.0573507304308743,-0.376415807126822));
#8710=CARTESIAN_POINT('Ctrl Pts',(3.09790240054779,-0.0124194594819549,
-0.371968696998067));
#8711=CARTESIAN_POINT('Ctrl Pts',(3.10076112917571,-0.0819474062969565,
-0.36752158686931));
#8712=CARTESIAN_POINT('Ctrl Pts',(3.10362479340891,-0.151595393363038,-0.363066798788869));
#8713=CARTESIAN_POINT('Ctrl Pts',(3.1101396997005,-0.220999815604975,-0.358612010708428));
#8714=CARTESIAN_POINT('Ctrl Pts',(3.12023419720762,-0.289755755186719,-0.354157222627986));
#8715=CARTESIAN_POINT('Ctrl Pts',(3.12535791437412,-0.32465456889044,-0.35189608242316));
#8716=CARTESIAN_POINT('Ctrl Pts',(3.13140303511768,-0.35938648889242,-0.349634942218332));
#8717=CARTESIAN_POINT('Ctrl Pts',(3.13835525008304,-0.393899974369568,-0.347373802013506));
#8718=CARTESIAN_POINT('Ctrl Pts',(3.15205435267856,-0.461907620973757,-0.342918302319794));
#8719=CARTESIAN_POINT('Ctrl Pts',(3.16933235935426,-0.529333367387134,-0.338462802626082));
#8720=CARTESIAN_POINT('Ctrl Pts',(3.19012476562827,-0.595772417517969,-0.33400730293237));
#8721=CARTESIAN_POINT('Ctrl Pts',(3.21088608116992,-0.66211212182518,-0.329558465514623));
#8722=CARTESIAN_POINT('Ctrl Pts',(3.23515122109042,-0.727467595143257,-0.325109628096875));
#8723=CARTESIAN_POINT('Ctrl Pts',(3.26280474150934,-0.791444554050085,-0.320660790679127));
#8724=CARTESIAN_POINT('Ctrl Pts',(3.29042589507674,-0.855346631614569,-0.316217160369116));
#8725=CARTESIAN_POINT('Ctrl Pts',(3.32142735900801,-0.917872952512026,-0.311773530059105));
#8726=CARTESIAN_POINT('Ctrl Pts',(3.35564456335289,-0.978646432078394,-0.307329899749094));
#8727=CARTESIAN_POINT('Ctrl Pts',(3.38984037203086,-1.03938191061133,-0.302889047995538));
#8728=CARTESIAN_POINT('Ctrl Pts',(3.4272476926212,-1.09836629688919,-0.298448196241982));
#8729=CARTESIAN_POINT('Ctrl Pts',(3.46765539455952,-1.15524584681022,-0.294007344488427));
#8730=CARTESIAN_POINT('Ctrl Pts',(3.50805153417745,-1.21210912113159,-0.289567763446847));
#8731=CARTESIAN_POINT('Ctrl Pts',(3.55144606756506,-1.2668683561977,-0.285128182405269));
#8732=CARTESIAN_POINT('Ctrl Pts',(3.5975847807408,-1.31919912015406,-0.280688601363689));
#8733=CARTESIAN_POINT('Ctrl Pts',(3.64372593908497,-1.37153265743295,-0.276248785041958));
#8734=CARTESIAN_POINT('Ctrl Pts',(3.69261124062395,-1.42143710277521,-0.271808968720226));
#8735=CARTESIAN_POINT('Ctrl Pts',(3.74394764538402,-1.46862278029303,-0.267369152398495));
#8736=CARTESIAN_POINT('Ctrl Pts',(3.79533823960252,-1.5158582658627,-0.262924649514798));
#8737=CARTESIAN_POINT('Ctrl Pts',(3.84918474015865,-1.56036892405346,-0.258480146631104));
#8738=CARTESIAN_POINT('Ctrl Pts',(3.90515957752016,-1.60190416432164,-0.254035643747407));
#8739=CARTESIAN_POINT('Ctrl Pts',(3.96116725097647,-1.64346377009316,-0.249588533618655));
#8740=CARTESIAN_POINT('Ctrl Pts',(4.01930533862264,-1.68204421326344,-0.245141423489901));
#8741=CARTESIAN_POINT('Ctrl Pts',(4.07921805092624,-1.71743876965416,-0.240694313361148));
#8742=CARTESIAN_POINT('Ctrl Pts',(4.13923420274386,-1.75289443487422,-0.236239525280709));
#8743=CARTESIAN_POINT('Ctrl Pts',(4.20103066145826,-1.785153007705,-0.23178473720027));
#8744=CARTESIAN_POINT('Ctrl Pts',(4.26422860847048,-1.81405452325566,-0.227329949119831));
#8745=CARTESIAN_POINT('Ctrl Pts',(4.29630632266763,-1.82872421743922,-0.225068808914983));
#8746=CARTESIAN_POINT('Ctrl Pts',(4.32874481068465,-1.84252980496825,-0.222807668710136));
#8747=CARTESIAN_POINT('Ctrl Pts',(4.36149303308618,-1.85545527990223,-0.220546528505288));
#8748=CARTESIAN_POINT('Ctrl Pts',(4.42602228897526,-1.88092448764353,-0.216091028811574));
#8749=CARTESIAN_POINT('Ctrl Pts',(4.4920085461044,-1.90307340780185,-0.21163552911786));
#8750=CARTESIAN_POINT('Ctrl Pts',(4.55907697268545,-1.92173614331675,-0.207180029424146));
#8751=CARTESIAN_POINT('Ctrl Pts',(4.62604511234083,-1.94037097258032,-0.2027311920064));
#8752=CARTESIAN_POINT('Ctrl Pts',(4.69409174222398,-1.95552983366991,-0.198282354588654));
#8753=CARTESIAN_POINT('Ctrl Pts',(4.76282316475469,-1.96709530034559,-0.193833517170908));
#8754=CARTESIAN_POINT('Ctrl Pts',(4.8314741411175,-1.97864723030925,-0.189389886860896));
#8755=CARTESIAN_POINT('Ctrl Pts',(4.90080783809015,-1.98661403863874,-0.184946256550884));
#8756=CARTESIAN_POINT('Ctrl Pts',(4.97041829000542,-1.99092888231321,-0.180502626240873));
#8757=CARTESIAN_POINT('Ctrl Pts',(5.0399852152191,-1.99524102796018,-0.176061774487317));
#8758=CARTESIAN_POINT('Ctrl Pts',(5.10982806494276,-1.99590570893784,-0.171620922733762));
#8759=CARTESIAN_POINT('Ctrl Pts',(5.17953515512022,-1.99290785067776,-0.167180070980206));
#8760=CARTESIAN_POINT('Ctrl Pts',(5.24922229920643,-1.98991085022934,-0.162740489938626));
#8761=CARTESIAN_POINT('Ctrl Pts',(5.31877327238994,-1.9832534121198,-0.158300908897045));
#8762=CARTESIAN_POINT('Ctrl Pts',(5.38777757473776,-1.9729725577165,-0.153861327855465));
#8763=CARTESIAN_POINT('Ctrl Pts',(5.45678553403936,-1.96269115846878,-0.149421511533734));
#8764=CARTESIAN_POINT('Ctrl Pts',(5.5252462815185,-1.94878603617264,-0.144981695212005));
#8765=CARTESIAN_POINT('Ctrl Pts',(5.592757384843,-1.93134569373299,-0.140541878890275));
#8766=CARTESIAN_POINT('Ctrl Pts',(5.66033975124378,-1.91388694169265,-0.136097376006578));
#8767=CARTESIAN_POINT('Ctrl Pts',(5.72696999824245,-1.89288564412286,-0.131652873122878));
#8768=CARTESIAN_POINT('Ctrl Pts',(5.79225973045888,-1.8684805325908,-0.127208370239181));
#8769=CARTESIAN_POINT('Ctrl Pts',(5.85758776309628,-1.84406110447306,-0.122761260110429));
#8770=CARTESIAN_POINT('Ctrl Pts',(5.92157326705565,-1.81623408319097,-0.118314149981678));
#8771=CARTESIAN_POINT('Ctrl Pts',(5.98384932664628,-1.78518573187346,-0.113867039852925));
#8772=CARTESIAN_POINT('Ctrl Pts',(6.04623290607856,-1.75408377546535,-0.109412251772485));
#8773=CARTESIAN_POINT('Ctrl Pts',(6.10690072439177,-1.71974962844176,-0.104957463692044));
#8774=CARTESIAN_POINT('Ctrl Pts',(6.16551259547016,-1.682414300984,-0.100502675611604));
#8775=CARTESIAN_POINT('Ctrl Pts',(6.19526253099646,-1.66346381255416,-0.0982415354067602));
#8776=CARTESIAN_POINT('Ctrl Pts',(6.22448328231698,-1.6437407944253,-0.0959803952019159));
#8777=CARTESIAN_POINT('Ctrl Pts',(6.25313367068295,-1.62327938637982,-0.0937192549970725));
#8778=CARTESIAN_POINT('Ctrl Pts',(6.30919037597055,-1.58324505574795,-0.0892951589444203));
#8779=CARTESIAN_POINT('Ctrl Pts',(6.36328866553822,-1.54021934802962,-0.0848710628917686));
#8780=CARTESIAN_POINT('Ctrl Pts',(6.41508822762698,-1.49442187539462,-0.0804469668391166));
#8781=CARTESIAN_POINT('Ctrl Pts',(6.4676615397328,-1.44794030826531,-0.0759567863591415));
#8782=CARTESIAN_POINT('Ctrl Pts',(6.51786641192738,-1.39860370997102,-0.0714666058791641));
#8783=CARTESIAN_POINT('Ctrl Pts',(6.56537740272673,-1.34668757781787,-0.0669764253991891));
#8784=CARTESIAN_POINT('Ctrl Pts',(6.61206431068767,-1.29567193611596,-0.0625641275441112));
#8785=CARTESIAN_POINT('Ctrl Pts',(6.6561496902821,-1.24216591063384,-0.0581518296890356));
#8786=CARTESIAN_POINT('Ctrl Pts',(6.69735963513394,-1.18647003717272,-0.0537395318339575));
#8787=CARTESIAN_POINT('Ctrl Pts',(6.73854493269571,-1.13080747490272,-0.0493298729337603));
#8788=CARTESIAN_POINT('Ctrl Pts',(6.7768579111523,-1.0729580606177,-0.0449202140335616));
#8789=CARTESIAN_POINT('Ctrl Pts',(6.81206500521088,-1.01325527591017,-0.0405105551333644));
#8790=CARTESIAN_POINT('Ctrl Pts',(6.8472634151172,-0.953567217441383,-0.0361019839159287));
#8791=CARTESIAN_POINT('Ctrl Pts',(6.87935720924913,-0.892027123974326,-0.0316934126984937));
#8792=CARTESIAN_POINT('Ctrl Pts',(6.90815724295914,-0.828995715351019,-0.027284841481058));
#8793=CARTESIAN_POINT('Ctrl Pts',(6.93788239464903,-0.763939604604037,-0.0227346576342798));
#8794=CARTESIAN_POINT('Ctrl Pts',(6.96409828625227,-0.697295220640624,-0.0181844737875009));
#8795=CARTESIAN_POINT('Ctrl Pts',(6.98665028780398,-0.629482447839057,-0.0136342899407227));
#8796=CARTESIAN_POINT('Ctrl Pts',(7.0085260120177,-0.563703208130607,-0.0092205545689134));
#8797=CARTESIAN_POINT('Ctrl Pts',(7.02695442780144,-0.496825181044442,-0.00480681919710362));
#8798=CARTESIAN_POINT('Ctrl Pts',(7.04184558333137,-0.429245579064855,-0.000393083825294127));
#8799=CARTESIAN_POINT('Ctrl Pts',(7.05742726807003,-0.358532191464125,0.00422532425896908));
#8800=CARTESIAN_POINT('Ctrl Pts',(7.06913552823614,-0.287051180071464,0.00884373234323341));
#8801=CARTESIAN_POINT('Ctrl Pts',(7.07692790107709,-0.215264941887005,0.0134621404274968));
#8802=CARTESIAN_POINT('Ctrl Pts',(7.08472027391804,-0.143478703702551,0.0180805485117599));
#8803=CARTESIAN_POINT('Ctrl Pts',(7.08859680264803,-0.0713878568362601,
0.0226989565960213));
#8804=CARTESIAN_POINT('Ctrl Pts',(7.08857708048266,0.000546895438558494,
0.0273173646802842));
#8805=CARTESIAN_POINT('Origin',(5.09382715545311,0.,-6.77268258743872));
#8806=CARTESIAN_POINT('',(7.08574931755807,0.000877333601738076,0.985439685988923));
#8807=CARTESIAN_POINT('',(7.08799998082202,-0.00180011721095886,0.827317077323091));
#8808=CARTESIAN_POINT('',(7.08857715545311,8.3550772080578E-14,-6.77268258743872));
#8809=CARTESIAN_POINT('Ctrl Pts',(7.08857700753084,0.000768203024997985,
0.987067856572719));
#8810=CARTESIAN_POINT('Ctrl Pts',(7.08858933050406,-0.0312301726838211,
0.985115999279288));
#8811=CARTESIAN_POINT('Ctrl Pts',(7.08783171154698,-0.0632230386489601,
0.983143267450536));
#8812=CARTESIAN_POINT('Ctrl Pts',(7.08582640517304,-0.10520044196499,0.980521111364263));
#8813=CARTESIAN_POINT('Ctrl Pts',(7.08527231882626,-0.115214145691052,0.979893078406499));
#8814=CARTESIAN_POINT('Ctrl Pts',(7.0841520241521,-0.133024757699987,0.978771364884858));
#8815=CARTESIAN_POINT('Ctrl Pts',(7.08361544695922,-0.140823369208531,0.978278609708121));
#8816=CARTESIAN_POINT('Ctrl Pts',(7.08245151287011,-0.156402210144011,0.977290972367816));
#8817=CARTESIAN_POINT('Ctrl Pts',(7.08182430136326,-0.164182311125906,0.976796103198259));
#8818=CARTESIAN_POINT('Ctrl Pts',(7.08038496486011,-0.180816727992611,0.975734435668629));
#8819=CARTESIAN_POINT('Ctrl Pts',(7.07955927011479,-0.189669670309279,0.975167223349754));
#8820=CARTESIAN_POINT('Ctrl Pts',(7.07722641219046,-0.212994494590406,0.973666882126047));
#8821=CARTESIAN_POINT('Ctrl Pts',(7.07562006848579,-0.227455704845281,0.972730673515336));
#8822=CARTESIAN_POINT('Ctrl Pts',(7.06803439242719,-0.289547460062802,0.968684232211899));
#8823=CARTESIAN_POINT('Ctrl Pts',(7.06049540021652,-0.336967820483085,0.965525760615543));
#8824=CARTESIAN_POINT('Ctrl Pts',(7.03874955882005,-0.447797169767986,0.957977989053789));
#8825=CARTESIAN_POINT('Ctrl Pts',(7.02314118997258,-0.510873300347682,0.953551498920586));
#8826=CARTESIAN_POINT('Ctrl Pts',(6.95640893442295,-0.733363187520309,0.937521287450869));
#8827=CARTESIAN_POINT('Ctrl Pts',(6.8883532505423,-0.886967348123215,0.925610988045209));
#8828=CARTESIAN_POINT('Ctrl Pts',(6.79399179646186,-1.04340939160515,0.91352171192033));
#8829=CARTESIAN_POINT('Ctrl Pts',(6.7859157462078,-1.05645596236879,0.912514397992516));
#8830=CARTESIAN_POINT('Ctrl Pts',(6.7742740563903,-1.07478666093634,0.911101763884265));
#8831=CARTESIAN_POINT('Ctrl Pts',(6.77083263355208,-1.08014850021139,0.910688887000755));
#8832=CARTESIAN_POINT('Ctrl Pts',(6.76487056722645,-1.08934039639549,0.909981774099608));
#8833=CARTESIAN_POINT('Ctrl Pts',(6.76236231640633,-1.09317839423996,0.909686735073077));
#8834=CARTESIAN_POINT('Ctrl Pts',(6.75745491332863,-1.1006312130914,0.909114265270557));
#8835=CARTESIAN_POINT('Ctrl Pts',(6.75505719229214,-1.10424686985238,0.908836739015987));
#8836=CARTESIAN_POINT('Ctrl Pts',(6.7484736346999,-1.11410460679468,0.908080558286499));
#8837=CARTESIAN_POINT('Ctrl Pts',(6.74426423540385,-1.12033097591016,0.907603452194914));
#8838=CARTESIAN_POINT('Ctrl Pts',(6.72787207223092,-1.14428468496136,0.905769336658876));
#8839=CARTESIAN_POINT('Ctrl Pts',(6.71543757080607,-1.16183905044525,0.904428145343044));
#8840=CARTESIAN_POINT('Ctrl Pts',(6.62109818806065,-1.29055629895297,0.894588147964476));
#8841=CARTESIAN_POINT('Ctrl Pts',(6.52812236524608,-1.39316166472405,0.886693171431795));
#8842=CARTESIAN_POINT('Ctrl Pts',(6.3612172466165,-1.54277408394262,0.873659216233273));
#8843=CARTESIAN_POINT('Ctrl Pts',(6.29350915655238,-1.59599214914898,0.868621600466437));
#8844=CARTESIAN_POINT('Ctrl Pts',(6.19616101741754,-1.66280319583515,0.861501493332392));
#8845=CARTESIAN_POINT('Ctrl Pts',(6.16930838452484,-1.68029591886193,0.859549952475419));
#8846=CARTESIAN_POINT('Ctrl Pts',(6.12808169278104,-1.70575922916512,0.856564380963674));
#8847=CARTESIAN_POINT('Ctrl Pts',(6.11401068859891,-1.71421192687885,0.855547217671982));
#8848=CARTESIAN_POINT('Ctrl Pts',(6.08787919982655,-1.72947387034107,0.853660539173462));
#8849=CARTESIAN_POINT('Ctrl Pts',(6.07584896049266,-1.73633305972348,0.852792850501278));
#8850=CARTESIAN_POINT('Ctrl Pts',(6.05818042832948,-1.74616463451512,0.851519363036846));
#8851=CARTESIAN_POINT('Ctrl Pts',(6.05259758309059,-1.7492362422812,0.851117096240894));
#8852=CARTESIAN_POINT('Ctrl Pts',(6.04009706425186,-1.75603604041251,0.850216607511358));
#8853=CARTESIAN_POINT('Ctrl Pts',(6.03317191333847,-1.75975019206691,0.849717899072887));
#8854=CARTESIAN_POINT('Ctrl Pts',(6.01795902973239,-1.76779389953994,0.848622598668168));
#8855=CARTESIAN_POINT('Ctrl Pts',(6.0096624723894,-1.77210627775708,0.848025416819078));
#8856=CARTESIAN_POINT('Ctrl Pts',(5.98690064656054,-1.78373486509993,0.846387289583115));
#8857=CARTESIAN_POINT('Ctrl Pts',(5.97237628243857,-1.79093320236204,0.845342273931895));
#8858=CARTESIAN_POINT('Ctrl Pts',(5.89536697714466,-1.82793712914644,0.839801682783555));
#8859=CARTESIAN_POINT('Ctrl Pts',(5.83145620865386,-1.8546486793968,0.835201608660842));
#8860=CARTESIAN_POINT('Ctrl Pts',(5.62644295420648,-1.92805953393274,0.820440128352348));
#8861=CARTESIAN_POINT('Ctrl Pts',(5.48144298219736,-1.96235556190953,0.80995367117517));
#8862=CARTESIAN_POINT('Ctrl Pts',(5.26767490901941,-1.9882828992491,0.795097658815514));
#8863=CARTESIAN_POINT('Ctrl Pts',(5.20097514536843,-1.99299101370848,0.790553546167207));
#8864=CARTESIAN_POINT('Ctrl Pts',(5.1239422999561,-1.99454883392951,0.785497343036555));
#8865=CARTESIAN_POINT('Ctrl Pts',(5.11372455186526,-1.99467693551602,0.784830592702827));
#8866=CARTESIAN_POINT('Ctrl Pts',(5.09809808085482,-1.99475275864742,0.783817337421511));
#8867=CARTESIAN_POINT('Ctrl Pts',(5.09268998530334,-1.99475700711887,0.783467843307091));
#8868=CARTESIAN_POINT('Ctrl Pts',(5.08278608712546,-1.99472450968177,0.782830052056166));
#8869=CARTESIAN_POINT('Ctrl Pts',(5.07829042772335,-1.99469455948538,0.782541394241501));
#8870=CARTESIAN_POINT('Ctrl Pts',(5.06819200070896,-1.99459314032741,0.781894892319105));
#8871=CARTESIAN_POINT('Ctrl Pts',(5.06258941940835,-1.99451326450462,0.781537517341971));
#8872=CARTESIAN_POINT('Ctrl Pts',(5.04617466811118,-1.99421005738547,0.780494083514686));
#8873=CARTESIAN_POINT('Ctrl Pts',(5.03536368767618,-1.99392240263961,0.7798114699834));
#8874=CARTESIAN_POINT('Ctrl Pts',(4.94707989597268,-1.99085471342288,0.774270910373587));
#8875=CARTESIAN_POINT('Ctrl Pts',(4.86981751251485,-1.98364811129229,0.769633299231163));
#8876=CARTESIAN_POINT('Ctrl Pts',(4.76900055770527,-1.96827655985396,0.763637456767907));
#8877=CARTESIAN_POINT('Ctrl Pts',(4.74490795980959,-1.96414876383731,0.762208956312499));
#8878=CARTESIAN_POINT('Ctrl Pts',(4.62076477469177,-1.94052290456797,0.754845453550176));
#8879=CARTESIAN_POINT('Ctrl Pts',(4.52224323688292,-1.91382038714486,0.748983722388977));
#8880=CARTESIAN_POINT('Ctrl Pts',(4.3765906672322,-1.86208763549841,0.739844790245944));
#8881=CARTESIAN_POINT('Ctrl Pts',(4.32770641704029,-1.84251375999521,0.736693940895876));
#8882=CARTESIAN_POINT('Ctrl Pts',(4.24812590021483,-1.80693381427013,0.731377947360863));
#8883=CARTESIAN_POINT('Ctrl Pts',(4.21696894987898,-1.79202117429641,0.729247488087762));
#8884=CARTESIAN_POINT('Ctrl Pts',(4.17512609362116,-1.77064141506663,0.726311037434362));
#8885=CARTESIAN_POINT('Ctrl Pts',(4.16408952991408,-1.76487126959923,0.72552923771205));
#8886=CARTESIAN_POINT('Ctrl Pts',(4.14566614664093,-1.75501837121576,0.724211571744321));
#8887=CARTESIAN_POINT('Ctrl Pts',(4.13824980314967,-1.75099134839588,0.723677677806174));
#8888=CARTESIAN_POINT('Ctrl Pts',(4.12368086677061,-1.74296039242088,0.722621911625202));
#8889=CARTESIAN_POINT('Ctrl Pts',(4.11652695371705,-1.73895918968645,0.722100144261402));
#8890=CARTESIAN_POINT('Ctrl Pts',(4.10084471896527,-1.73006073780542,0.72094888675366));
#8891=CARTESIAN_POINT('Ctrl Pts',(4.09232758368497,-1.72514430634191,0.720318717642497));
#8892=CARTESIAN_POINT('Ctrl Pts',(4.06256597544102,-1.70767003927824,0.718099162861348));
#8893=CARTESIAN_POINT('Ctrl Pts',(4.04151921849765,-1.69478154935099,0.716497893791444));
#8894=CARTESIAN_POINT('Ctrl Pts',(3.89457901009348,-1.6010067511858,0.705087663659892));
#8895=CARTESIAN_POINT('Ctrl Pts',(3.77792111874581,-1.50658361087159,0.69475971840475));
#8896=CARTESIAN_POINT('Ctrl Pts',(3.61303446982983,-1.33924019962458,0.678381243629311));
#8897=CARTESIAN_POINT('Ctrl Pts',(3.55709443014078,-1.27466286401111,0.672427474676137));
#8898=CARTESIAN_POINT('Ctrl Pts',(3.48981916624115,-1.18610896681386,0.664884785239939));
#8899=CARTESIAN_POINT('Ctrl Pts',(3.47457874721772,-1.16521707575679,0.663147262203817));
#8900=CARTESIAN_POINT('Ctrl Pts',(3.44980002268579,-1.12982442012886,0.660280431883248));
#8901=CARTESIAN_POINT('Ctrl Pts',(3.44003726457693,-1.11548531111601,0.659139328091417));
#8902=CARTESIAN_POINT('Ctrl Pts',(3.42677010260964,-1.09544196281118,0.657574253910239));
#8903=CARTESIAN_POINT('Ctrl Pts',(3.42310581638526,-1.08984518240066,0.657140421393751));
#8904=CARTESIAN_POINT('Ctrl Pts',(3.41694593465387,-1.08033258437424,0.656408583271429));
#8905=CARTESIAN_POINT('Ctrl Pts',(3.41443574970077,-1.07642632326586,0.656109627980898));
#8906=CARTESIAN_POINT('Ctrl Pts',(3.40964993606804,-1.06892131818717,0.655538301422917));
#8907=CARTESIAN_POINT('Ctrl Pts',(3.40737216849611,-1.06532402045757,0.655265783233808));
#8908=CARTESIAN_POINT('Ctrl Pts',(3.40194818500458,-1.05669688600632,0.654615330133348));
#8909=CARTESIAN_POINT('Ctrl Pts',(3.3988128340925,-1.05166021701891,0.654238099889289));
#8910=CARTESIAN_POINT('Ctrl Pts',(3.38760148493088,-1.03346976879617,0.65288444572383));
#8911=CARTESIAN_POINT('Ctrl Pts',(3.37965550819028,-1.02023595291727,0.65191604332005));
#8912=CARTESIAN_POINT('Ctrl Pts',(3.304928558915,-0.892442028525047,0.642707489967446));
#8913=CARTESIAN_POINT('Ctrl Pts',(3.24956440567278,-0.771567186257269,0.635075328255049));
#8914=CARTESIAN_POINT('Ctrl Pts',(3.16174589489612,-0.515044827721414,0.619332800805632));
#8915=CARTESIAN_POINT('Ctrl Pts',(3.13066181454087,-0.379716056752711,0.611245451444885));
#8916=CARTESIAN_POINT('Ctrl Pts',(3.1114862375932,-0.222999696529675,0.601470774210416));
#8917=CARTESIAN_POINT('Ctrl Pts',(3.10941007728325,-0.203698792149985,0.600260704707658));
#8918=CARTESIAN_POINT('Ctrl Pts',(3.10669835558373,-0.174485701038683,0.598418478188881));
#8919=CARTESIAN_POINT('Ctrl Pts',(3.10585455797687,-0.164593660582055,0.597792820940868));
#8920=CARTESIAN_POINT('Ctrl Pts',(3.10446203099679,-0.146691582730595,0.596657025150946));
#8921=CARTESIAN_POINT('Ctrl Pts',(3.10388774767208,-0.138683701777267,0.596147695761916));
#8922=CARTESIAN_POINT('Ctrl Pts',(3.10275874292916,-0.121486189425074,0.595051052305967));
#8923=CARTESIAN_POINT('Ctrl Pts',(3.10221926949032,-0.11229577673031,0.594463274439087));
#8924=CARTESIAN_POINT('Ctrl Pts',(3.10093822586508,-0.0875441320799671,
0.592875463044831));
#8925=CARTESIAN_POINT('Ctrl Pts',(3.10031531586669,-0.0719776590437602,
0.591871762972886));
#8926=CARTESIAN_POINT('Ctrl Pts',(3.09815180318625,0.0045027353531572,0.58691424663997));
#8927=CARTESIAN_POINT('Ctrl Pts',(3.09922065736666,0.0654522681362345,0.582880450135189));
#8928=CARTESIAN_POINT('Ctrl Pts',(3.11398924657116,0.298323779092428,0.567145057156788));
#8929=CARTESIAN_POINT('Ctrl Pts',(3.14716716388484,0.468248884516733,0.554906658301742));
#8930=CARTESIAN_POINT('Ctrl Pts',(3.21865593293446,0.682353377977116,0.539441611548483));
#8931=CARTESIAN_POINT('Ctrl Pts',(3.23757538508093,0.732259319725125,0.535841133344036));
#8932=CARTESIAN_POINT('Ctrl Pts',(3.26227854851062,0.790285745881826,0.531706517414003));
#8933=CARTESIAN_POINT('Ctrl Pts',(3.26614754188102,0.799192779633129,0.5310733437841));
#8934=CARTESIAN_POINT('Ctrl Pts',(3.2722285820963,0.812917148938568,0.53010042354739));
#8935=CARTESIAN_POINT('Ctrl Pts',(3.2743949798016,0.817754372213337,0.529758035496906));
#8936=CARTESIAN_POINT('Ctrl Pts',(3.27843757834327,0.826685262209806,0.529126935881807));
#8937=CARTESIAN_POINT('Ctrl Pts',(3.28030835103319,0.830781190271786,0.528837915582169));
#8938=CARTESIAN_POINT('Ctrl Pts',(3.28459371740461,0.840080252108739,0.528182668327269));
#8939=CARTESIAN_POINT('Ctrl Pts',(3.28701689168331,0.845279324270073,0.527816970778189));
#8940=CARTESIAN_POINT('Ctrl Pts',(3.29338296313067,0.858785670227963,0.526868455338145));
#8941=CARTESIAN_POINT('Ctrl Pts',(3.29736098714569,0.867076369626628,0.526287712332161));
#8942=CARTESIAN_POINT('Ctrl Pts',(3.32468672233866,0.923031223800151,0.522376362590108));
#8943=CARTESIAN_POINT('Ctrl Pts',(3.34987358980212,0.969779122122044,0.51914864448852));
#8944=CARTESIAN_POINT('Ctrl Pts',(3.40403769129978,1.06135827035434,0.512796574315339));
#8945=CARTESIAN_POINT('Ctrl Pts',(3.43300767941705,1.10614148658201,0.509675215368583));
#8946=CARTESIAN_POINT('Ctrl Pts',(3.46646291681158,1.15357511447568,0.506295635134601));
#8947=CARTESIAN_POINT('Ctrl Pts',(3.46920131922337,1.15742853012372,0.506020542850604));
#8948=CARTESIAN_POINT('Ctrl Pts',(3.53984361356951,1.25609005430591,0.498962361133775));
#8949=CARTESIAN_POINT('Ctrl Pts',(3.61591376547616,1.34476668441478,0.492250380324655));
#8950=CARTESIAN_POINT('Ctrl Pts',(3.72732247486301,1.45369505229739,0.48292690179726));
#8951=CARTESIAN_POINT('Ctrl Pts',(3.75615302617345,1.48026754011568,0.480554907324072));
#8952=CARTESIAN_POINT('Ctrl Pts',(3.80668964077068,1.52416341503441,0.476447089226139));
#8953=CARTESIAN_POINT('Ctrl Pts',(3.82800916317559,1.54191497525253,0.474728503231998));
#8954=CARTESIAN_POINT('Ctrl Pts',(3.85863613430209,1.5663529805301,0.472275666010715));
#8955=CARTESIAN_POINT('Ctrl Pts',(3.86764223140399,1.57341318212586,0.47155629866383));
#8956=CARTESIAN_POINT('Ctrl Pts',(3.88323713766525,1.58542337437207,0.470313640984269));
#8957=CARTESIAN_POINT('Ctrl Pts',(3.88979685633321,1.59041079682835,0.469791836538894));
#8958=CARTESIAN_POINT('Ctrl Pts',(3.90239466325912,1.59986643197529,0.468791332550558));
#8959=CARTESIAN_POINT('Ctrl Pts',(3.9084274682486,1.6043414732104,0.468312910852757));
#8960=CARTESIAN_POINT('Ctrl Pts',(3.92415832427271,1.61587321154236,0.467067116136874));
#8961=CARTESIAN_POINT('Ctrl Pts',(3.93389488746113,1.62287662307256,0.466297710979303));
#8962=CARTESIAN_POINT('Ctrl Pts',(3.96208379917769,1.64276935341432,0.464074618630753));
#8963=CARTESIAN_POINT('Ctrl Pts',(3.98069143837439,1.65543437801828,0.462612548269991));
#8964=CARTESIAN_POINT('Ctrl Pts',(4.1185324620018,1.74587906234593,0.451817389919458));
#8965=CARTESIAN_POINT('Ctrl Pts',(4.24555351083098,1.81099736871511,0.442017271612711));
#8966=CARTESIAN_POINT('Ctrl Pts',(4.48674195265708,1.90366674384796,0.424009238702443));
#8967=CARTESIAN_POINT('Ctrl Pts',(4.59852427816608,1.93576318956978,0.415887783591245));
#8968=CARTESIAN_POINT('Ctrl Pts',(4.73094737885038,1.9615555416094,0.406918458820201));
#8969=CARTESIAN_POINT('Ctrl Pts',(4.74947420859436,1.96489261407854,0.40567841748981));
#8970=CARTESIAN_POINT('Ctrl Pts',(4.77486026315743,1.9690950679872,0.404001987608267));
#8971=CARTESIAN_POINT('Ctrl Pts',(4.78168017386383,1.97018768913885,0.403553850334167));
#8972=CARTESIAN_POINT('Ctrl Pts',(4.79313720605387,1.97196224149596,0.402804906332139));
#8973=CARTESIAN_POINT('Ctrl Pts',(4.79777125658616,1.97266328442418,0.402503048148923));
#8974=CARTESIAN_POINT('Ctrl Pts',(4.80657726369382,1.97396373463445,0.401931515785278));
#8975=CARTESIAN_POINT('Ctrl Pts',(4.81074870473869,1.97456626060287,0.401661662978566));
#8976=CARTESIAN_POINT('Ctrl Pts',(4.82172924761074,1.9761167861845,0.400953577408447));
#8977=CARTESIAN_POINT('Ctrl Pts',(4.82854146718782,1.97704282477957,0.400516564026644));
#8978=CARTESIAN_POINT('Ctrl Pts',(4.85246627418038,1.98016922577878,0.39898930705221));
#8979=CARTESIAN_POINT('Ctrl Pts',(4.86960305301516,1.98218284640876,0.397908912076251));
#8980=CARTESIAN_POINT('Ctrl Pts',(5.08690571252716,2.00486221309185,0.384355771215339));
#8981=CARTESIAN_POINT('Ctrl Pts',(5.28908317093018,1.99535015550772,0.373219953486289));
#8982=CARTESIAN_POINT('Ctrl Pts',(5.55844915347913,1.94127488704387,0.356921542620261));
#8983=CARTESIAN_POINT('Ctrl Pts',(5.6295973500766,1.92285472482053,0.352483673434621));
#8984=CARTESIAN_POINT('Ctrl Pts',(5.71477497335138,1.89570733033441,0.346925318252895));
#8985=CARTESIAN_POINT('Ctrl Pts',(5.72992789989978,1.89067667636234,0.345926946017115));
#8986=CARTESIAN_POINT('Ctrl Pts',(5.75371585769108,1.88246092413269,0.344343807939059));
#8987=CARTESIAN_POINT('Ctrl Pts',(5.7623922383161,1.87939696595334,0.343763027837884));
#8988=CARTESIAN_POINT('Ctrl Pts',(5.77859905554735,1.87354729620979,0.342671749511088));
#8989=CARTESIAN_POINT('Ctrl Pts',(5.78613449904791,1.87077592597892,0.342161734989936));
#8990=CARTESIAN_POINT('Ctrl Pts',(5.80295594601757,1.86447381717529,0.341017254691192));
#8991=CARTESIAN_POINT('Ctrl Pts',(5.81223266609789,1.86091906673445,0.340381999937955));
#8992=CARTESIAN_POINT('Ctrl Pts',(5.83571199729209,1.85172028338359,0.338763570870283));
#8993=CARTESIAN_POINT('Ctrl Pts',(5.84987680765042,1.84598213110689,0.337777273468373));
#8994=CARTESIAN_POINT('Ctrl Pts',(5.9372083701089,1.80943042988531,0.331633431469182));
#8995=CARTESIAN_POINT('Ctrl Pts',(6.00853832505779,1.77443822790524,0.326335532534088));
#8996=CARTESIAN_POINT('Ctrl Pts',(6.19895626974579,1.66648791979571,0.311412832064357));
#8997=CARTESIAN_POINT('Ctrl Pts',(6.31276890968104,1.58513981081485,0.301566077684162));
#8998=CARTESIAN_POINT('Ctrl Pts',(6.46561006475343,1.44963220491833,0.287487060666978));
#8999=CARTESIAN_POINT('Ctrl Pts',(6.51195452894013,1.40432846317499,0.283087468987644));
#9000=CARTESIAN_POINT('Ctrl Pts',(6.56292253644513,1.349403349098,0.278170898965221));
#9001=CARTESIAN_POINT('Ctrl Pts',(6.56977165177564,1.34190852564304,0.277508489135789));
#9002=CARTESIAN_POINT('Ctrl Pts',(6.5801717762404,1.33035195638334,0.276500438671891));
#9003=CARTESIAN_POINT('Ctrl Pts',(6.58376390907266,1.32632768630837,0.276151854861484));
#9004=CARTESIAN_POINT('Ctrl Pts',(6.59032031333211,1.31892229053519,0.275514941508939));
#9005=CARTESIAN_POINT('Ctrl Pts',(6.59328947449365,1.31554571742619,0.275226257883646));
#9006=CARTESIAN_POINT('Ctrl Pts',(6.59994345340446,1.30792692145483,0.274578728297315));
#9007=CARTESIAN_POINT('Ctrl Pts',(6.60362177345716,1.30367915842826,0.27422035870733));
#9008=CARTESIAN_POINT('Ctrl Pts',(6.61437490586963,1.29115477527212,0.273171285709451));
#9009=CARTESIAN_POINT('Ctrl Pts',(6.62140009252877,1.28283555043032,0.272484083755965));
#9010=CARTESIAN_POINT('Ctrl Pts',(6.69210067218446,1.19770754798058,0.265544488935228));
#9011=CARTESIAN_POINT('Ctrl Pts',(6.7500055793617,1.11627063992951,0.259659780319202));
#9012=CARTESIAN_POINT('Ctrl Pts',(6.86656164731685,0.92317534566154,0.246510170043034));
#9013=CARTESIAN_POINT('Ctrl Pts',(6.92121678538167,0.809620980763616,0.239301175932445));
#9014=CARTESIAN_POINT('Ctrl Pts',(6.98567245401892,0.635268419905961,0.228183968001383));
#9015=CARTESIAN_POINT('Ctrl Pts',(7.00396305018982,0.577948450553578,0.224525631253163));
#9016=CARTESIAN_POINT('Ctrl Pts',(7.02356493823274,0.505338447638272,0.219843908597162));
#9017=CARTESIAN_POINT('Ctrl Pts',(7.02732905994982,0.49073946514589,0.218900323853748));
#9018=CARTESIAN_POINT('Ctrl Pts',(7.033077004583,0.467352875729911,0.217384533140573));
#9019=CARTESIAN_POINT('Ctrl Pts',(7.03516745732663,0.458591883741971,0.216815752055405));
#9020=CARTESIAN_POINT('Ctrl Pts',(7.03901510331051,0.441968673891558,0.215734628264384));
#9021=CARTESIAN_POINT('Ctrl Pts',(7.04078414526777,0.434109361674526,0.215222676144252));
#9022=CARTESIAN_POINT('Ctrl Pts',(7.04469197690292,0.416243574058273,0.21405698053053));
#9023=CARTESIAN_POINT('Ctrl Pts',(7.0468014622848,0.406230987177652,0.213402318075054));
#9024=CARTESIAN_POINT('Ctrl Pts',(7.05206423375543,0.380262584027074,0.211700668782033));
#9025=CARTESIAN_POINT('Ctrl Pts',(7.05509952453204,0.364283894837235,0.210649981332873));
#9026=CARTESIAN_POINT('Ctrl Pts',(7.07832854179385,0.233281068275994,0.202004230086555));
#9027=CARTESIAN_POINT('Ctrl Pts',(7.0885771554597,0.116744612167536,0.19409417477583));
#9028=CARTESIAN_POINT('Ctrl Pts',(7.08857715545311,-1.12589937373286E-10,
0.186011338956534));
#9029=CARTESIAN_POINT('Ctrl Pts',(7.09164130412058,0.000548482472640843,
0.0273174125612813));
#9030=CARTESIAN_POINT('Ctrl Pts',(7.09175165964625,0.0306588665693442,0.0292476145445689));
#9031=CARTESIAN_POINT('Ctrl Pts',(7.07750675584133,0.720147590609536,0.0734535743639286));
#9032=CARTESIAN_POINT('Ctrl Pts',(6.28353627797873,2.03415344877187,0.159935292019361));
#9033=CARTESIAN_POINT('Ctrl Pts',(4.03314932025975,2.10431712897573,0.286762565527578));
#9034=CARTESIAN_POINT('Ctrl Pts',(2.75099003209035,0.253578908358813,0.413589839035793));
#9035=CARTESIAN_POINT('Ctrl Pts',(3.60746290235971,-1.82863592781539,0.540417112544011));
#9036=CARTESIAN_POINT('Ctrl Pts',(5.82074643570099,-2.24160130473173,0.667244386052225));
#9037=CARTESIAN_POINT('Ctrl Pts',(6.98930590305859,-1.01005560487751,0.762877707645254));
#9038=CARTESIAN_POINT('Ctrl Pts',(7.0895351504061,-0.175492384774626,0.816235271402208));
#9039=CARTESIAN_POINT('Ctrl Pts',(7.08799998082202,-0.00180011721095886,
0.827317077323091));
#9040=CARTESIAN_POINT('Origin',(5.09382715545311,0.,-6.77268258743872));
#9041=CARTESIAN_POINT('',(7.09089099632987,0.00118553966962425,1.78540654381999));
#9042=CARTESIAN_POINT('',(7.08857697543044,0.000847467636836062,1.62559580930988));
#9043=CARTESIAN_POINT('',(7.08857715545311,8.3550772080578E-14,-6.77268258743872));
#9044=CARTESIAN_POINT('Ctrl Pts',(7.08569498022126,0.000879430672124808,
0.98540839880601));
#9045=CARTESIAN_POINT('Ctrl Pts',(7.08678274233512,0.277777209942647,1.00302338867406));
#9046=CARTESIAN_POINT('Ctrl Pts',(6.90380563625223,1.21784867470375,1.06291413637816));
#9047=CARTESIAN_POINT('Ctrl Pts',(5.46844469401115,2.32655315630881,1.16508064191835));
#9048=CARTESIAN_POINT('Ctrl Pts',(3.34465355126974,1.57910721350831,1.29190791542657));
#9049=CARTESIAN_POINT('Ctrl Pts',(2.81757559157258,-0.609808746458473,1.41873518893479));
#9050=CARTESIAN_POINT('Ctrl Pts',(4.36834792145259,-2.24206774437344,1.545562462443));
#9051=CARTESIAN_POINT('Ctrl Pts',(6.50103911243751,-1.84272189433612,1.66778624740474));
#9052=CARTESIAN_POINT('Ctrl Pts',(7.08669410382909,-0.587071448118138,1.7477342745304));
#9053=CARTESIAN_POINT('Ctrl Pts',(7.09089099632987,0.00118553966962425,
1.78540654381999));
#9054=CARTESIAN_POINT('Ctrl Pts',(7.0885763647563,-0.00177608679726875,
0.826985646114236));
#9055=CARTESIAN_POINT('Ctrl Pts',(7.08868588521213,0.121227948264429,0.834139298127843));
#9056=CARTESIAN_POINT('Ctrl Pts',(7.07741849588526,0.243966340480971,0.841373813191014));
#9057=CARTESIAN_POINT('Ctrl Pts',(7.05234424202085,0.37873053609996,0.849854099289273));
#9058=CARTESIAN_POINT('Ctrl Pts',(7.04962091607336,0.392551586002556,0.850729931092804));
#9059=CARTESIAN_POINT('Ctrl Pts',(7.04483881375989,0.415534874801099,0.852197153040885));
#9060=CARTESIAN_POINT('Ctrl Pts',(7.04286128675278,0.424713636800601,0.85278599318071));
#9061=CARTESIAN_POINT('Ctrl Pts',(7.03885051903425,0.442711628765464,0.853946447802865));
#9062=CARTESIAN_POINT('Ctrl Pts',(7.03682191146503,0.451531665422038,0.854517903215624));
#9063=CARTESIAN_POINT('Ctrl Pts',(7.03287599886028,0.468168690931863,0.855601194125967));
#9064=CARTESIAN_POINT('Ctrl Pts',(7.03097126152878,0.475988497217635,0.85611261786743));
#9065=CARTESIAN_POINT('Ctrl Pts',(7.02655505248188,0.493653390368693,0.857273118556198));
#9066=CARTESIAN_POINT('Ctrl Pts',(7.0240155952107,0.503491186129817,0.857923082986224));
#9067=CARTESIAN_POINT('Ctrl Pts',(7.01727740638661,0.52879438030944,0.859604479214082));
#9068=CARTESIAN_POINT('Ctrl Pts',(7.01296733037436,0.544229114153417,0.860639466959637));
#9069=CARTESIAN_POINT('Ctrl Pts',(6.9802897750228,0.6560318371411,0.868206274058423));
#9070=CARTESIAN_POINT('Ctrl Pts',(6.94486879863639,0.750172200959767,0.874967460973669));
#9071=CARTESIAN_POINT('Ctrl Pts',(6.86897249869979,0.913352553146966,0.887357286841124));
#9072=CARTESIAN_POINT('Ctrl Pts',(6.83114694016992,0.983398676253002,0.892915225182642));
#9073=CARTESIAN_POINT('Ctrl Pts',(6.7457906570638,1.12109121095605,0.904198058605296));
#9074=CARTESIAN_POINT('Ctrl Pts',(6.69802961713367,1.18842991395529,0.909910786085606));
#9075=CARTESIAN_POINT('Ctrl Pts',(6.63098309168,1.27152229034517,0.917055776786366));
#9076=CARTESIAN_POINT('Ctrl Pts',(6.61538860095439,1.29014270609605,0.91866336862861));
#9077=CARTESIAN_POINT('Ctrl Pts',(6.59570283851815,1.31279463438316,0.92062229974999));
#9078=CARTESIAN_POINT('Ctrl Pts',(6.59192991242095,1.31709849704309,0.920994645150306));
#9079=CARTESIAN_POINT('Ctrl Pts',(6.58459339276969,1.32539512136817,0.921712608816385));
#9080=CARTESIAN_POINT('Ctrl Pts',(6.58103215601027,1.32938989390171,0.922058388856411));
#9081=CARTESIAN_POINT('Ctrl Pts',(6.57444765594131,1.33671640046393,0.922692635044146));
#9082=CARTESIAN_POINT('Ctrl Pts',(6.57142920746619,1.34005222971507,0.922981434857892));
#9083=CARTESIAN_POINT('Ctrl Pts',(6.56458099061302,1.3475692435902,0.923632294358708));
#9084=CARTESIAN_POINT('Ctrl Pts',(6.56074467006493,1.35174432387743,0.923993854523405));
#9085=CARTESIAN_POINT('Ctrl Pts',(6.55078880798085,1.36248702210499,0.924924504355055));
#9086=CARTESIAN_POINT('Ctrl Pts',(6.54464256510118,1.36902987423392,0.925491645721486));
#9087=CARTESIAN_POINT('Ctrl Pts',(6.50478428292887,1.41089026656067,0.92912402867857));
#9088=CARTESIAN_POINT('Ctrl Pts',(6.4698263874983,1.44500461267795,0.932102313942063));
#9089=CARTESIAN_POINT('Ctrl Pts',(6.42479674488353,1.48582982815332,0.935743528451845));
#9090=CARTESIAN_POINT('Ctrl Pts',(6.41587276406192,1.49377566706049,0.936456066889964));
#9091=CARTESIAN_POINT('Ctrl Pts',(6.39518527671644,1.51186502349082,0.938088563889319));
#9092=CARTESIAN_POINT('Ctrl Pts',(6.38337355393024,1.52195233509276,0.939006585551655));
#9093=CARTESIAN_POINT('Ctrl Pts',(6.27208436503667,1.61476843457911,0.947538457978001));
#9094=CARTESIAN_POINT('Ctrl Pts',(6.16489763445384,1.68777261484291,0.954910765022636));
#9095=CARTESIAN_POINT('Ctrl Pts',(6.00527918727699,1.77511863148812,0.965669602161265));
#9096=CARTESIAN_POINT('Ctrl Pts',(5.95818750901853,1.79851926391426,0.968816309368003));
#9097=CARTESIAN_POINT('Ctrl Pts',(5.88907081627617,1.82952256855478,0.973435991059897));
#9098=CARTESIAN_POINT('Ctrl Pts',(5.86774938100145,1.83864342170898,0.974861134518082));
#9099=CARTESIAN_POINT('Ctrl Pts',(5.82939159871417,1.8542666547606,0.977428271221079));
#9100=CARTESIAN_POINT('Ctrl Pts',(5.81241576623851,1.86091113472771,0.978565513292725));
#9101=CARTESIAN_POINT('Ctrl Pts',(5.78618747575369,1.87076470600111,0.980325383990736));
#9102=CARTESIAN_POINT('Ctrl Pts',(5.77699818656824,1.87413999880106,0.980942486878824));
#9103=CARTESIAN_POINT('Ctrl Pts',(5.76023605057662,1.88015719277037,0.982069248550743));
#9104=CARTESIAN_POINT('Ctrl Pts',(5.7526713649376,1.88282133767239,0.982578158905946));
#9105=CARTESIAN_POINT('Ctrl Pts',(5.73628839733822,1.88848030020195,0.983681288950033));
#9106=CARTESIAN_POINT('Ctrl Pts',(5.72746482732273,1.89145911600715,0.984276021662022));
#9107=CARTESIAN_POINT('Ctrl Pts',(5.7033830829423,1.89940163740608,0.985901009224233));
#9108=CARTESIAN_POINT('Ctrl Pts',(5.68808562198402,1.90424311972026,0.986935227127497));
#9109=CARTESIAN_POINT('Ctrl Pts',(5.6083402182553,1.92842720330545,0.99233804363489));
#9110=CARTESIAN_POINT('Ctrl Pts',(5.5430088348754,1.94468230016142,0.996805127362824));
#9111=CARTESIAN_POINT('Ctrl Pts',(5.32520107462839,1.98731358011449,1.01183187748595));
#9112=CARTESIAN_POINT('Ctrl Pts',(5.1704806266177,1.99926599218372,1.02276545288767));
#9113=CARTESIAN_POINT('Ctrl Pts',(4.95285332191976,1.99076433039015,1.03776580876369));
#9114=CARTESIAN_POINT('Ctrl Pts',(4.88989111252952,1.98530300523955,1.04205238743651));
#9115=CARTESIAN_POINT('Ctrl Pts',(4.81728024913999,1.97551293365793,1.04685940784675));
#9116=CARTESIAN_POINT('Ctrl Pts',(4.80728243225285,1.97408755487096,1.04751824048855));
#9117=CARTESIAN_POINT('Ctrl Pts',(4.79197268023666,1.9717860969947,1.04852199936756));
#9118=CARTESIAN_POINT('Ctrl Pts',(4.78665292169807,1.9709643650444,1.04886983110966));
#9119=CARTESIAN_POINT('Ctrl Pts',(4.7768950503948,1.96941662069338,1.04950602353467));
#9120=CARTESIAN_POINT('Ctrl Pts',(4.77245607308137,1.96869713599838,1.04979473283966));
#9121=CARTESIAN_POINT('Ctrl Pts',(4.7624627727306,1.9670426866259,1.05044313095317));
#9122=CARTESIAN_POINT('Ctrl Pts',(4.75690996183444,1.9660992069719,1.05080233730861));
#9123=CARTESIAN_POINT('Ctrl Pts',(4.74057325746439,1.96325218933645,1.05185616520005));
#9124=CARTESIAN_POINT('Ctrl Pts',(4.72980075185064,1.96128332109259,1.0525472376041));
#9125=CARTESIAN_POINT('Ctrl Pts',(4.62539700811044,1.94131181532914,1.05921248716136));
#9126=CARTESIAN_POINT('Ctrl Pts',(4.53314083208464,1.91670397416537,1.06485158582226));
#9127=CARTESIAN_POINT('Ctrl Pts',(4.32090679316549,1.84344820613787,1.07795806450416));
#9128=CARTESIAN_POINT('Ctrl Pts',(4.20321119964475,1.78955563110373,1.08534972944516));
#9129=CARTESIAN_POINT('Ctrl Pts',(4.0388540677999,1.69404080767417,1.09671272475468));
#9130=CARTESIAN_POINT('Ctrl Pts',(3.98759227486737,1.66101949795878,1.10041870225073));
#9131=CARTESIAN_POINT('Ctrl Pts',(3.92558875594306,1.61693405840853,1.10515413976605));
#9132=CARTESIAN_POINT('Ctrl Pts',(3.91335231108198,1.60802233482565,1.1061014975676));
#9133=CARTESIAN_POINT('Ctrl Pts',(3.89398807404771,1.59357933872107,1.10762192721523));
#9134=CARTESIAN_POINT('Ctrl Pts',(3.88679417305922,1.58813736974165,1.10819153670643));
#9135=CARTESIAN_POINT('Ctrl Pts',(3.8732477905546,1.57774473097067,1.10927332532144));
#9136=CARTESIAN_POINT('Ctrl Pts',(3.86688788106388,1.5728040043109,1.10978510727268));
#9137=CARTESIAN_POINT('Ctrl Pts',(3.85253358663092,1.56151275240015,1.11094916213402));
#9138=CARTESIAN_POINT('Ctrl Pts',(3.8445577380757,1.555139130859,1.11160234408242));
#9139=CARTESIAN_POINT('Ctrl Pts',(3.82406251242802,1.53850167011593,1.11329760302683));
#9140=CARTESIAN_POINT('Ctrl Pts',(3.81161872439032,1.52814631216959,1.11434333470068));
#9141=CARTESIAN_POINT('Ctrl Pts',(3.69886261633687,1.43196707372869,1.12397309232721));
#9142=CARTESIAN_POINT('Ctrl Pts',(3.60719428583301,1.33655026569795,1.13296646418753));
#9143=CARTESIAN_POINT('Ctrl Pts',(3.46360618589662,1.15389776730633,1.14911250125984));
#9144=CARTESIAN_POINT('Ctrl Pts',(3.40762141382675,1.07042586172218,1.15615824221394));
#9145=CARTESIAN_POINT('Ctrl Pts',(3.33324494159126,0.939112720499902,1.1664801153287));
#9146=CARTESIAN_POINT('Ctrl Pts',(3.31001220405886,0.894196627364318,1.16988600621986));
#9147=CARTESIAN_POINT('Ctrl Pts',(3.28443485263501,0.839773073438701,1.17382740609879));
#9148=CARTESIAN_POINT('Ctrl Pts',(3.28042293007745,0.83107427138136,1.17445187390053));
#9149=CARTESIAN_POINT('Ctrl Pts',(3.27430041537561,0.817543757974525,1.17541430968631));
#9150=CARTESIAN_POINT('Ctrl Pts',(3.27214611711516,0.812732151555461,1.17575483197036));
#9151=CARTESIAN_POINT('Ctrl Pts',(3.2681858941751,0.803792169150238,1.17638424198223));
#9152=CARTESIAN_POINT('Ctrl Pts',(3.26637489307639,0.799666240014152,1.17667342461088));
#9153=CARTESIAN_POINT('Ctrl Pts',(3.26227486617728,0.790238647117166,1.17733126997386));
#9154=CARTESIAN_POINT('Ctrl Pts',(3.2599948719872,0.784933160130323,1.17769938588998));
#9155=CARTESIAN_POINT('Ctrl Pts',(3.25409378739322,0.77103542923949,1.17865839010778));
#9156=CARTESIAN_POINT('Ctrl Pts',(3.25050979584178,0.762427451199525,1.17924712749256));
#9157=CARTESIAN_POINT('Ctrl Pts',(3.22578006475225,0.701838150012314,1.18335649095078));
#9158=CARTESIAN_POINT('Ctrl Pts',(3.20677370348674,0.649004804328121,1.1867619785163));
#9159=CARTESIAN_POINT('Ctrl Pts',(3.14153607493148,0.440418054127619,1.19977972615778));
#9160=CARTESIAN_POINT('Ctrl Pts',(3.11216579189744,0.280057282763585,1.2089310684923));
#9161=CARTESIAN_POINT('Ctrl Pts',(3.09858391442029,0.0506725858960808,1.22261140241009));
#9162=CARTESIAN_POINT('Ctrl Pts',(3.0980108666019,-0.0167097643938952,1.22669320503519));
#9163=CARTESIAN_POINT('Ctrl Pts',(3.10150236903982,-0.0995615022827879,
1.23185164631077));
#9164=CARTESIAN_POINT('Ctrl Pts',(3.10234120635525,-0.115127061154027,1.23282674717197));
#9165=CARTESIAN_POINT('Ctrl Pts',(3.10395977710108,-0.139780314017471,1.23438128418566));
#9166=CARTESIAN_POINT('Ctrl Pts',(3.10461957050992,-0.148875448515927,1.23495697723747));
#9167=CARTESIAN_POINT('Ctrl Pts',(3.10597826079827,-0.165978764400661,1.23604382022391));
#9168=CARTESIAN_POINT('Ctrl Pts',(3.10666324956169,-0.173987891092742,1.23655452537729));
#9169=CARTESIAN_POINT('Ctrl Pts',(3.1083138179867,-0.192003679451014,1.23770736845103));
#9170=CARTESIAN_POINT('Ctrl Pts',(3.10930666819829,-0.202007563601819,1.23835034707886));
#9171=CARTESIAN_POINT('Ctrl Pts',(3.11204063916505,-0.227585932798022,1.24000175797526));
#9172=CARTESIAN_POINT('Ctrl Pts',(3.11388973105284,-0.243147949275802,1.24101353688902));
#9173=CARTESIAN_POINT('Ctrl Pts',(3.12750631684129,-0.347259863561881,1.24783117968266));
#9174=CARTESIAN_POINT('Ctrl Pts',(3.1450255154403,-0.434942856405148,1.25381650631273));
#9175=CARTESIAN_POINT('Ctrl Pts',(3.20246250893086,-0.647153923318922,1.26887880832107));
#9176=CARTESIAN_POINT('Ctrl Pts',(3.24885120636143,-0.769499210961667,1.27808571170147));
#9177=CARTESIAN_POINT('Ctrl Pts',(3.33491077256789,-0.94298803141268,1.29142382870392));
#9178=CARTESIAN_POINT('Ctrl Pts',(3.36563801139996,-0.998186977223847,1.29570875444621));
#9179=CARTESIAN_POINT('Ctrl Pts',(3.40425965363882,-1.06042028597661,1.30051417019413));
#9180=CARTESIAN_POINT('Ctrl Pts',(3.4096494230972,-1.06895972898002,1.30117294928082));
#9181=CARTESIAN_POINT('Ctrl Pts',(3.4180113242286,-1.08198790865894,1.30217664389418));
#9182=CARTESIAN_POINT('Ctrl Pts',(3.42093707257289,-1.08650600868829,1.30252446436339));
#9183=CARTESIAN_POINT('Ctrl Pts',(3.42634069087662,-1.09477699812055,1.30316064601167));
#9184=CARTESIAN_POINT('Ctrl Pts',(3.42881295903287,-1.09853334572575,1.30344935573086));
#9185=CARTESIAN_POINT('Ctrl Pts',(3.43441045278032,-1.10697583275807,1.30409776699518));
#9186=CARTESIAN_POINT('Ctrl Pts',(3.43754283127734,-1.11165710845368,1.30445698599538));
#9187=CARTESIAN_POINT('Ctrl Pts',(3.44682380083002,-1.12540101558673,1.30551088581962));
#9188=CARTESIAN_POINT('Ctrl Pts',(3.45302736014259,-1.13442652493345,1.30620201678799));
#9189=CARTESIAN_POINT('Ctrl Pts',(3.51469158211374,-1.22257718702694,1.31294758963633));
#9190=CARTESIAN_POINT('Ctrl Pts',(3.57576585207085,-1.29763596365087,1.31865777531509));
#9191=CARTESIAN_POINT('Ctrl Pts',(3.72992466539398,-1.46123813505024,1.33177479200388));
#9192=CARTESIAN_POINT('Ctrl Pts',(3.82657750061869,-1.54580855188678,1.3391121715747));
#9193=CARTESIAN_POINT('Ctrl Pts',(3.97999522860306,-1.65592633917945,1.35040223775383));
#9194=CARTESIAN_POINT('Ctrl Pts',(4.03090428074749,-1.68905520510378,1.3540942315785));
#9195=CARTESIAN_POINT('Ctrl Pts',(4.09627689004247,-1.72746914139894,1.3588139050938));
#9196=CARTESIAN_POINT('Ctrl Pts',(4.10939894780213,-1.7349804756009,1.35976016172238));
#9197=CARTESIAN_POINT('Ctrl Pts',(4.13048041244361,-1.74673178023111,1.36127923750642));
#9198=CARTESIAN_POINT('Ctrl Pts',(4.13838554503755,-1.75106829795945,1.36184860526043));
#9199=CARTESIAN_POINT('Ctrl Pts',(4.1534073220118,-1.75917678766124,1.36293019928703));
#9200=CARTESIAN_POINT('Ctrl Pts',(4.16051796093685,-1.76295955078381,1.36344203030652));
#9201=CARTESIAN_POINT('Ctrl Pts',(4.17669951808578,-1.77144258485193,1.36460656106286));
#9202=CARTESIAN_POINT('Ctrl Pts',(4.18578397209565,-1.77611641099654,1.36526017271778));
#9203=CARTESIAN_POINT('Ctrl Pts',(4.20937507982432,-1.78802541175428,1.36695728561161));
#9204=CARTESIAN_POINT('Ctrl Pts',(4.22393451538618,-1.79515378624694,1.36800445482687));
#9205=CARTESIAN_POINT('Ctrl Pts',(4.3561196040296,-1.85788661773408,1.37751181064768));
#9206=CARTESIAN_POINT('Ctrl Pts',(4.47881396472044,-1.90202589465157,1.38636873105349));
#9207=CARTESIAN_POINT('Ctrl Pts',(4.69501908764519,-1.9566855956825,1.40186051902902));
#9208=CARTESIAN_POINT('Ctrl Pts',(4.78661181556632,-1.97314103692516,1.40838099060096));
#9209=CARTESIAN_POINT('Ctrl Pts',(4.93785018435352,-1.98952267502758,1.41883742924191));
#9210=CARTESIAN_POINT('Ctrl Pts',(4.99694223377235,-1.99327470206726,1.42284488258068));
#9211=CARTESIAN_POINT('Ctrl Pts',(5.06607120701462,-1.99458172255865,1.42737992105554));
#9212=CARTESIAN_POINT('Ctrl Pts',(5.07602474636018,-1.99469539646983,1.42802917776658));
#9213=CARTESIAN_POINT('Ctrl Pts',(5.09133097324201,-1.9947556181219,1.42902143887776));
#9214=CARTESIAN_POINT('Ctrl Pts',(5.09668312232891,-1.99475513585723,1.42936724897319));
#9215=CARTESIAN_POINT('Ctrl Pts',(5.10653401486099,-1.99471460043362,1.43000152344635));
#9216=CARTESIAN_POINT('Ctrl Pts',(5.11103261183845,-1.99468087033309,1.43029032170984));
#9217=CARTESIAN_POINT('Ctrl Pts',(5.1212001710391,-1.99457023479798,1.43094114414589));
#9218=CARTESIAN_POINT('Ctrl Pts',(5.12686893598415,-1.99448438102811,1.43130266905137));
#9219=CARTESIAN_POINT('Ctrl Pts',(5.14151042168657,-1.99420019434433,1.43223316704755));
#9220=CARTESIAN_POINT('Ctrl Pts',(5.15048242131318,-1.99396547034398,1.43280019289785));
#9221=CARTESIAN_POINT('Ctrl Pts',(5.20821349402025,-1.99206513865789,1.43643015098726));
#9222=CARTESIAN_POINT('Ctrl Pts',(5.25690345640201,-1.98867159853613,1.43940625996395));
#9223=CARTESIAN_POINT('Ctrl Pts',(5.31727077717616,-1.98223168462877,1.44304330572243));
#9224=CARTESIAN_POINT('Ctrl Pts',(5.32910608160495,-1.9808617667577,1.44375381807446));
#9225=CARTESIAN_POINT('Ctrl Pts',(5.38519704842794,-1.97385951536751,1.44711192356172));
#9226=CARTESIAN_POINT('Ctrl Pts',(5.42926927204036,-1.96684942625532,1.449723412437));
#9227=CARTESIAN_POINT('Ctrl Pts',(5.57133357311861,-1.93933825542637,1.45815151630666));
#9228=CARTESIAN_POINT('Ctrl Pts',(5.66802211307992,-1.91294141462753,1.46391060009365));
#9229=CARTESIAN_POINT('Ctrl Pts',(5.81198757905177,-1.86173363410699,1.47294461755129));
#9230=CARTESIAN_POINT('Ctrl Pts',(5.86093208789885,-1.84210638622161,1.47609981891295));
#9231=CARTESIAN_POINT('Ctrl Pts',(5.94059422850549,-1.8064352845173,1.48142245761996));
#9232=CARTESIAN_POINT('Ctrl Pts',(5.97177475682855,-1.79148840389108,1.48355509354209));
#9233=CARTESIAN_POINT('Ctrl Pts',(6.01364066590578,-1.77006380954949,1.48649407898795));
#9234=CARTESIAN_POINT('Ctrl Pts',(6.02467793756905,-1.76428444252867,1.48727618153017));
#9235=CARTESIAN_POINT('Ctrl Pts',(6.04310029392587,-1.75441708486186,1.4885942148425));
#9236=CARTESIAN_POINT('Ctrl Pts',(6.05051497491265,-1.75038487528702,1.48912817085473));
#9237=CARTESIAN_POINT('Ctrl Pts',(6.06507902621646,-1.74234455315991,1.49018394878059));
#9238=CARTESIAN_POINT('Ctrl Pts',(6.07222972927428,-1.73833918975679,1.49070566511893));
#9239=CARTESIAN_POINT('Ctrl Pts',(6.08790301718155,-1.72943268072501,1.49185667499705));
#9240=CARTESIAN_POINT('Ctrl Pts',(6.09641442112615,-1.72451239051302,1.49248664640925));
#9241=CARTESIAN_POINT('Ctrl Pts',(6.12614594634335,-1.70703062531568,1.49470476312118));
#9242=CARTESIAN_POINT('Ctrl Pts',(6.14716848577829,-1.69413918955307,1.49630477140708));
#9243=CARTESIAN_POINT('Ctrl Pts',(6.29419952297177,-1.6001821549085,1.50772621058428));
#9244=CARTESIAN_POINT('Ctrl Pts',(6.41093886649239,-1.50554892768608,1.51806815817619));
#9245=CARTESIAN_POINT('Ctrl Pts',(6.57572230825244,-1.3380120299621,1.53445124953916));
#9246=CARTESIAN_POINT('Ctrl Pts',(6.63152695485236,-1.27348747834946,1.54039579366242));
#9247=CARTESIAN_POINT('Ctrl Pts',(6.69864955264566,-1.18500634576088,1.54792809271975));
#9248=CARTESIAN_POINT('Ctrl Pts',(6.71386268603432,-1.16412197641763,1.54966408729761));
#9249=CARTESIAN_POINT('Ctrl Pts',(6.73859881770702,-1.12874010624515,1.55252866853464));
#9250=CARTESIAN_POINT('Ctrl Pts',(6.74834591273059,-1.11440377736808,1.55366902934093));
#9251=CARTESIAN_POINT('Ctrl Pts',(6.76159302367388,-1.09436250737981,1.55523326308586));
#9252=CARTESIAN_POINT('Ctrl Pts',(6.76525276526315,-1.08876476923418,1.55566698456514));
#9253=CARTESIAN_POINT('Ctrl Pts',(6.77140541001005,-1.07924988687978,1.55639869056438));
#9254=CARTESIAN_POINT('Ctrl Pts',(6.77391289650791,-1.07534228169564,1.55669762398468));
#9255=CARTESIAN_POINT('Ctrl Pts',(6.77869389049834,-1.06783415335291,1.55726895192234));
#9256=CARTESIAN_POINT('Ctrl Pts',(6.7809695338261,-1.06423507264721,1.55754149310483));
#9257=CARTESIAN_POINT('Ctrl Pts',(6.78638888899157,-1.05560293404586,1.55819205759979));
#9258=CARTESIAN_POINT('Ctrl Pts',(6.7895217228161,-1.0505630454944,1.55856937569974));
#9259=CARTESIAN_POINT('Ctrl Pts',(6.80072717755369,-1.03235576239227,1.55992373592898));
#9260=CARTESIAN_POINT('Ctrl Pts',(6.8086695410251,-1.01910830260573,1.56089274540703));
#9261=CARTESIAN_POINT('Ctrl Pts',(6.88317644899737,-0.891496690866052,1.57008446312052));
#9262=CARTESIAN_POINT('Ctrl Pts',(6.93836908015773,-0.770851691292086,1.57770181565766));
#9263=CARTESIAN_POINT('Ctrl Pts',(7.01224746100827,-0.554876411634715,1.5909546887953));
#9264=CARTESIAN_POINT('Ctrl Pts',(7.03670053823518,-0.462023181029013,1.59653848531472));
#9265=CARTESIAN_POINT('Ctrl Pts',(7.06068877438946,-0.334146345189335,1.60436519464526));
#9266=CARTESIAN_POINT('Ctrl Pts',(7.06613089193132,-0.300360091902404,1.60644484331557));
#9267=CARTESIAN_POINT('Ctrl Pts',(7.074040471966,-0.241676923280253,1.61008855110985));
#9268=CARTESIAN_POINT('Ctrl Pts',(7.0769136057831,-0.216842242814626,1.61164023631095));
#9269=CARTESIAN_POINT('Ctrl Pts',(7.08037599207359,-0.181030062406835,1.61389450174166));
#9270=CARTESIAN_POINT('Ctrl Pts',(7.08134250711003,-0.170090808104385,1.61458532230418));
#9271=CARTESIAN_POINT('Ctrl Pts',(7.08286965505979,-0.151010213238009,1.61579438933496));
#9272=CARTESIAN_POINT('Ctrl Pts',(7.08347075439294,-0.142872305672123,1.61631136111081));
#9273=CARTESIAN_POINT('Ctrl Pts',(7.08453639539062,-0.127131069107989,1.61731395542222));
#9274=CARTESIAN_POINT('Ctrl Pts',(7.08500735027745,-0.119528305453479,1.61779936839217));
#9275=CARTESIAN_POINT('Ctrl Pts',(7.08602425914138,-0.101432996149796,1.61895757754274));
#9276=CARTESIAN_POINT('Ctrl Pts',(7.08653087790814,-0.0909385517432676,
1.61963158787929));
#9277=CARTESIAN_POINT('Ctrl Pts',(7.08804761812425,-0.0533573980563534,
1.62205376793542));
#9278=CARTESIAN_POINT('Ctrl Pts',(7.08858849018638,-0.026255737248853,1.6238163996891));
#9279=CARTESIAN_POINT('Ctrl Pts',(7.08857697543068,0.000847466486712864,
1.62559580923438));
#9280=CARTESIAN_POINT('Origin',(5.09382715545311,0.,-6.77268258743872));
#9281=CARTESIAN_POINT('',(7.08857715545311,-4.46037469243765E-12,2.58513735103561));
#9282=CARTESIAN_POINT('',(7.08857715545311,3.31900585956301E-12,2.42843892255116));
#9283=CARTESIAN_POINT('',(7.08857715545311,8.3550772080578E-14,-6.77268258743872));
#9284=CARTESIAN_POINT('Ctrl Pts',(7.08857715545311,-4.46037469243765E-12,
2.58513735103561));
#9285=CARTESIAN_POINT('Ctrl Pts',(7.08857715545311,-0.000573719608935291,
2.58509735546341));
#9286=CARTESIAN_POINT('Ctrl Pts',(7.08857690794817,-0.00114744621619411,
2.5850573598134));
#9287=CARTESIAN_POINT('Ctrl Pts',(7.08848669686533,-0.105696979192502,2.5777690776299));
#9288=CARTESIAN_POINT('Ctrl Pts',(7.0802675235093,-0.209517219190061,2.57053655223239));
#9289=CARTESIAN_POINT('Ctrl Pts',(7.06143895699791,-0.328324287216113,2.56256261290403));
#9290=CARTESIAN_POINT('Ctrl Pts',(7.05869142175094,-0.344385677503512,2.56149132306044));
#9291=CARTESIAN_POINT('Ctrl Pts',(7.05453409991877,-0.367016247174239,2.55999303130221));
#9292=CARTESIAN_POINT('Ctrl Pts',(7.05328755290711,-0.373614241838874,2.55955754629472));
#9293=CARTESIAN_POINT('Ctrl Pts',(7.05113055116343,-0.384723481594506,2.55882672037121));
#9294=CARTESIAN_POINT('Ctrl Pts',(7.05023776523568,-0.38923806029832,2.55853040052529));
#9295=CARTESIAN_POINT('Ctrl Pts',(7.04837726867743,-0.398477955800474,2.55792536341682));
#9296=CARTESIAN_POINT('Ctrl Pts',(7.04740803185068,-0.40320291037588,2.55761673401851));
#9297=CARTESIAN_POINT('Ctrl Pts',(7.04487923356733,-0.415307403405743,2.55682793516335));
#9298=CARTESIAN_POINT('Ctrl Pts',(7.04329492154234,-0.422681776465845,2.55634914865173));
#9299=CARTESIAN_POINT('Ctrl Pts',(7.03654530011051,-0.45325329490668,2.55437095749661));
#9300=CARTESIAN_POINT('Ctrl Pts',(7.0310072414085,-0.476367264709833,2.5528913307589));
#9301=CARTESIAN_POINT('Ctrl Pts',(7.01507216005735,-0.537992550662144,2.54897599316184));
#9302=CARTESIAN_POINT('Ctrl Pts',(7.00393064837729,-0.576301476716016,2.54657321417147));
#9303=CARTESIAN_POINT('Ctrl Pts',(6.96302695915687,-0.702679160232502,2.53867397384158));
#9304=CARTESIAN_POINT('Ctrl Pts',(6.9282601985986,-0.78900125435267,2.5333190285089));
#9305=CARTESIAN_POINT('Ctrl Pts',(6.83068645720054,-0.989582874354239,2.52035413885513));
#9306=CARTESIAN_POINT('Ctrl Pts',(6.76247293712642,-1.10071311236439,2.51271335222203));
#9307=CARTESIAN_POINT('Ctrl Pts',(6.67414690560076,-1.21732482860213,2.50364148351342));
#9308=CARTESIAN_POINT('Ctrl Pts',(6.66420405110684,-1.23012464107434,2.50263055900577));
#9309=CARTESIAN_POINT('Ctrl Pts',(6.64774199701153,-1.25079198175833,2.500972511094));
#9310=CARTESIAN_POINT('Ctrl Pts',(6.64131625733275,-1.25873324806766,2.50032908520142));
#9311=CARTESIAN_POINT('Ctrl Pts',(6.62971568100584,-1.27284675782588,2.49917397885932));
#9312=CARTESIAN_POINT('Ctrl Pts',(6.62456388861122,-1.27903771738645,2.49866323334785));
#9313=CARTESIAN_POINT('Ctrl Pts',(6.61356524242223,-1.29209326901283,2.49757743981052));
#9314=CARTESIAN_POINT('Ctrl Pts',(6.6077090676292,-1.29894973744654,2.49700201819154));
#9315=CARTESIAN_POINT('Ctrl Pts',(6.59190776114077,-1.31719806337294,2.49545642952337));
#9316=CARTESIAN_POINT('Ctrl Pts',(6.58187939399751,-1.32851674955159,2.49448284069538));
#9317=CARTESIAN_POINT('Ctrl Pts',(6.53092557945538,-1.38472584832802,2.48957130630115));
#9318=CARTESIAN_POINT('Ctrl Pts',(6.48809716165513,-1.42784012020302,2.48555347849539));
#9319=CARTESIAN_POINT('Ctrl Pts',(6.34890602483313,-1.55571872228121,2.47281711541159));
#9320=CARTESIAN_POINT('Ctrl Pts',(6.24629634363261,-1.63318451950424,2.46384730766719));
#9321=CARTESIAN_POINT('Ctrl Pts',(6.05475870269731,-1.7506976620583,2.44820626857386));
#9322=CARTESIAN_POINT('Ctrl Pts',(5.9689803915567,-1.79511641088729,2.44154495567969));
#9323=CARTESIAN_POINT('Ctrl Pts',(5.87025165707929,-1.83747448335675,2.43448380087461));
#9324=CARTESIAN_POINT('Ctrl Pts',(5.86015226473081,-1.84170934828089,2.43376834075116));
#9325=CARTESIAN_POINT('Ctrl Pts',(5.84480627547875,-1.84799611670255,2.4326921022895));
#9326=CARTESIAN_POINT('Ctrl Pts',(5.8395852131858,-1.85010924198218,2.43232783858872));
#9327=CARTESIAN_POINT('Ctrl Pts',(5.83017962902903,-1.85386968784311,2.43167512630488));
#9328=CARTESIAN_POINT('Ctrl Pts',(5.8259984441861,-1.85552499039581,2.43138621184632));
#9329=CARTESIAN_POINT('Ctrl Pts',(5.81680014102241,-1.85913060269655,2.43075335303533));
#9330=CARTESIAN_POINT('Ctrl Pts',(5.81178071873145,-1.86107474819246,2.43040977566365));
#9331=CARTESIAN_POINT('Ctrl Pts',(5.79732221245928,-1.86660768254147,2.42942500326855));
#9332=CARTESIAN_POINT('Ctrl Pts',(5.78786350363949,-1.87014520646106,2.42878676278455));
#9333=CARTESIAN_POINT('Ctrl Pts',(5.71906671136189,-1.89528111443893,2.42418514161373));
#9334=CARTESIAN_POINT('Ctrl Pts',(5.65875314684194,-1.91412521714479,2.42036849887057));
#9335=CARTESIAN_POINT('Ctrl Pts',(5.47119934078904,-1.96308295014561,2.40887262654789));
#9336=CARTESIAN_POINT('Ctrl Pts',(5.34181735192287,-1.98358464360659,2.40143621479675));
#9337=CARTESIAN_POINT('Ctrl Pts',(5.12233882242346,-1.99653855467507,2.38850345739401));
#9338=CARTESIAN_POINT('Ctrl Pts',(5.03308044899175,-1.99581713805682,2.38316097668914));
#9339=CARTESIAN_POINT('Ctrl Pts',(4.92855467919921,-1.98795321724429,2.37665573846926));
#9340=CARTESIAN_POINT('Ctrl Pts',(4.91294759723048,-1.98659395675224,2.37567805316845));
#9341=CARTESIAN_POINT('Ctrl Pts',(4.88735593673216,-1.98406104476503,2.37406370505062));
#9342=CARTESIAN_POINT('Ctrl Pts',(4.87736116652256,-1.98299547735774,2.37343041631689));
#9343=CARTESIAN_POINT('Ctrl Pts',(4.85938873959165,-1.98094189846097,2.37228640864415));
#9344=CARTESIAN_POINT('Ctrl Pts',(4.85140814392135,-1.97998110992984,2.37177655289128));
#9345=CARTESIAN_POINT('Ctrl Pts',(4.83438567337417,-1.97782730709113,2.37068496388786));
#9346=CARTESIAN_POINT('Ctrl Pts',(4.82534576313014,-1.97662046856116,2.37010280736916));
#9347=CARTESIAN_POINT('Ctrl Pts',(4.80087328572113,-1.97318238686339,2.36851999043552));
#9348=CARTESIAN_POINT('Ctrl Pts',(4.78545834529982,-1.97083214803336,2.36751561578986));
#9349=CARTESIAN_POINT('Ctrl Pts',(4.70354291555591,-1.95735836392356,2.36213782085551));
#9350=CARTESIAN_POINT('Ctrl Pts',(4.63761780627047,-1.9430503921944,2.35766501998584));
#9351=CARTESIAN_POINT('Ctrl Pts',(4.41527893604923,-1.8828560118263,2.34207818634153));
#9352=CARTESIAN_POINT('Ctrl Pts',(4.26382249444988,-1.82116901288849,2.3305323609567));
#9353=CARTESIAN_POINT('Ctrl Pts',(4.07304642713492,-1.71467892953277,2.31553700698514));
#9354=CARTESIAN_POINT('Ctrl Pts',(4.02566046045887,-1.68556763416592,2.31177793981085));
#9355=CARTESIAN_POINT('Ctrl Pts',(3.97183298482576,-1.64931597028355,2.30751837738337));
#9356=CARTESIAN_POINT('Ctrl Pts',(3.96415390008503,-1.64406582374947,2.30691097775461));
#9357=CARTESIAN_POINT('Ctrl Pts',(3.95177306966717,-1.63547341670854,2.30593248898806));
#9358=CARTESIAN_POINT('Ctrl Pts',(3.94704870530792,-1.63216421352643,2.30555930339028));
#9359=CARTESIAN_POINT('Ctrl Pts',(3.93865978803633,-1.62623375135579,2.30489708968436));
#9360=CARTESIAN_POINT('Ctrl Pts',(3.93498970032776,-1.62362052671022,2.30460753330765));
#9361=CARTESIAN_POINT('Ctrl Pts',(3.92704052122951,-1.61791976140729,2.30398072729817));
#9362=CARTESIAN_POINT('Ctrl Pts',(3.92276481898809,-1.61482767186317,2.30364379373602));
#9363=CARTESIAN_POINT('Ctrl Pts',(3.91074390443229,-1.60606156922683,2.30269696796216));
#9364=CARTESIAN_POINT('Ctrl Pts',(3.9030271914508,-1.60034846125837,2.30208968656104));
#9365=CARTESIAN_POINT('Ctrl Pts',(3.85458379453603,-1.56393873265297,2.29827856599865));
#9366=CARTESIAN_POINT('Ctrl Pts',(3.81500190856164,-1.53174261143752,2.29516995696243));
#9367=CARTESIAN_POINT('Ctrl Pts',(3.66307971639062,-1.39816886611485,2.28306543251376));
#9368=CARTESIAN_POINT('Ctrl Pts',(3.56119267277551,-1.28567172073096,2.27451550732722));
#9369=CARTESIAN_POINT('Ctrl Pts',(3.42513065256275,-1.09600338927351,2.26073953776204));
#9370=CARTESIAN_POINT('Ctrl Pts',(3.38143397847467,-1.02639109805841,2.25580258936769));
#9371=CARTESIAN_POINT('Ctrl Pts',(3.33478690212518,-0.940766759608716,2.24974907106564));
#9372=CARTESIAN_POINT('Ctrl Pts',(3.32757675490616,-0.927159215387747,2.24878774231288));
#9373=CARTESIAN_POINT('Ctrl Pts',(3.31595931342593,-0.904606491047544,2.24719492621851));
#9374=CARTESIAN_POINT('Ctrl Pts',(3.31146017417314,-0.895709163519963,2.24656665863416));
#9375=CARTESIAN_POINT('Ctrl Pts',(3.30345749830837,-0.879584310686831,2.24542806908599));
#9376=CARTESIAN_POINT('Ctrl Pts',(3.29993053373128,-0.872368601185418,2.24491857476578));
#9377=CARTESIAN_POINT('Ctrl Pts',(3.29246765359788,-0.856863877629572,2.24382373283922));
#9378=CARTESIAN_POINT('Ctrl Pts',(3.28854517631425,-0.848568636518223,2.24323793562943));
#9379=CARTESIAN_POINT('Ctrl Pts',(3.27800430532759,-0.825872939481146,2.24163492871836));
#9380=CARTESIAN_POINT('Ctrl Pts',(3.27150018904831,-0.811420445118591,2.24061384193927));
#9381=CARTESIAN_POINT('Ctrl Pts',(3.23661781731842,-0.731374587668034,2.23495557412002));
#9382=CARTESIAN_POINT('Ctrl Pts',(3.21161145830348,-0.664377380568385,2.23020614307114));
#9383=CARTESIAN_POINT('Ctrl Pts',(3.13074538170396,-0.406180303545514,2.21185322607464));
#9384=CARTESIAN_POINT('Ctrl Pts',(3.10002531576418,-0.208360686616569,2.19756165325407));
#9385=CARTESIAN_POINT('Ctrl Pts',(3.09900330149986,0.0112260014355715,2.18292509024981));
#9386=CARTESIAN_POINT('Ctrl Pts',(3.0992241727132,0.031737221718923,2.18157112332532));
#9387=CARTESIAN_POINT('Ctrl Pts',(3.09995457959188,0.0596165245670277,2.17975195303466));
#9388=CARTESIAN_POINT('Ctrl Pts',(3.10018868346224,0.0669897446255821,2.17927285375449));
#9389=CARTESIAN_POINT('Ctrl Pts',(3.10062439742731,0.0786696425545959,2.17851728627743));
#9390=CARTESIAN_POINT('Ctrl Pts',(3.1007990729447,0.0829771682582987,2.17823936138324));
#9391=CARTESIAN_POINT('Ctrl Pts',(3.1011890859604,0.0918818019196473,2.17766637784101));
#9392=CARTESIAN_POINT('Ctrl Pts',(3.10140636869013,0.09647875615187,2.17737144083562));
#9393=CARTESIAN_POINT('Ctrl Pts',(3.10196736203407,0.107535936348531,2.17666401576725));
#9394=CARTESIAN_POINT('Ctrl Pts',(3.10232659874164,0.113995393095449,2.1762523839259));
#9395=CARTESIAN_POINT('Ctrl Pts',(3.10367987786609,0.136365324376934,2.17483216710323));
#9396=CARTESIAN_POINT('Ctrl Pts',(3.10483324373412,0.152266033455754,2.17383198872394));
#9397=CARTESIAN_POINT('Ctrl Pts',(3.11300310290739,0.248838426580558,2.16780490114641));
#9398=CARTESIAN_POINT('Ctrl Pts',(3.12473665448713,0.329044153011078,2.16299934898406));
#9399=CARTESIAN_POINT('Ctrl Pts',(3.14335931388687,0.418093792678475,2.15767544688168));
#9400=CARTESIAN_POINT('Ctrl Pts',(3.14547613124226,0.427849867520452,2.15709235779567));
#9401=CARTESIAN_POINT('Ctrl Pts',(3.18494951883587,0.603406034773257,2.14659730859552));
#9402=CARTESIAN_POINT('Ctrl Pts',(3.2432656605022,0.763760633117595,2.13689461735431));
#9403=CARTESIAN_POINT('Ctrl Pts',(3.33287164656392,0.937395842272723,2.12488322039284));
#9404=CARTESIAN_POINT('Ctrl Pts',(3.34497421363898,0.959785687809845,2.12330493213328));
#9405=CARTESIAN_POINT('Ctrl Pts',(3.36253858954976,0.990844171914539,2.12107095219737));
#9406=CARTESIAN_POINT('Ctrl Pts',(3.36764415169489,0.999712209973037,2.12042789487105));
#9407=CARTESIAN_POINT('Ctrl Pts',(3.37663378895675,1.0150524487599,2.11930625250237));
#9408=CARTESIAN_POINT('Ctrl Pts',(3.38048681988609,1.02154266854423,2.11882879059802));
#9409=CARTESIAN_POINT('Ctrl Pts',(3.38860722345512,1.03504586217697,2.11782922766435));
#9410=CARTESIAN_POINT('Ctrl Pts',(3.39288123180449,1.04205466018784,2.11730689195173));
#9411=CARTESIAN_POINT('Ctrl Pts',(3.40312522985354,1.05862248937828,2.11606368430328));
#9412=CARTESIAN_POINT('Ctrl Pts',(3.40913315713055,1.06815761929625,2.11534143147613));
#9413=CARTESIAN_POINT('Ctrl Pts',(3.42963834521986,1.10009786666879,2.11289885138197));
#9414=CARTESIAN_POINT('Ctrl Pts',(3.44450380888544,1.12226204464093,2.11116496894654));
#9415=CARTESIAN_POINT('Ctrl Pts',(3.48117831717035,1.17464011011243,2.10697109318897));
#9416=CARTESIAN_POINT('Ctrl Pts',(3.50339742555177,1.2045532964318,2.10449634357187));
#9417=CARTESIAN_POINT('Ctrl Pts',(3.63306096163795,1.36927108110008,2.09041226106833));
#9418=CARTESIAN_POINT('Ctrl Pts',(3.75678498732379,1.49031695341213,2.0781989271691));
#9419=CARTESIAN_POINT('Ctrl Pts',(3.90465801102348,1.60158241139967,2.06547736257107));
#9420=CARTESIAN_POINT('Ctrl Pts',(3.91489880817895,1.60913561800787,2.06460537013808));
#9421=CARTESIAN_POINT('Ctrl Pts',(3.96316921555431,1.6440297755906,2.06053945428449));
#9422=CARTESIAN_POINT('Ctrl Pts',(4.00208523368305,1.67012623195947,2.05738841463674));
#9423=CARTESIAN_POINT('Ctrl Pts',(4.04942704916241,1.69951014410303,2.05373447625333));
#9424=CARTESIAN_POINT('Ctrl Pts',(4.05699818960729,1.7041396698787,2.05315541968772));
#9425=CARTESIAN_POINT('Ctrl Pts',(4.06943032267463,1.71162802232842,2.05221353495416));
#9426=CARTESIAN_POINT('Ctrl Pts',(4.07427289377631,1.71451697781279,2.05184885220961));
#9427=CARTESIAN_POINT('Ctrl Pts',(4.08299960641099,1.71967306587462,2.05119570073469));
#9428=CARTESIAN_POINT('Ctrl Pts',(4.08687920534985,1.72194762242423,2.05090676318343));
#9429=CARTESIAN_POINT('Ctrl Pts',(4.09541458688559,1.72691309011338,2.05027422045819));
#9430=CARTESIAN_POINT('Ctrl Pts',(4.10007356496417,1.72959830044494,2.04993097971947));
#9431=CARTESIAN_POINT('Ctrl Pts',(4.11349072492165,1.7372591937295,2.04894814375579));
#9432=CARTESIAN_POINT('Ctrl Pts',(4.12227596127596,1.74218750722841,2.04831148504797));
#9433=CARTESIAN_POINT('Ctrl Pts',(4.1857627619635,1.77717253870128,2.0437571747549));
#9434=CARTESIAN_POINT('Ctrl Pts',(4.24181691384659,1.80471698307592,2.03998284885645));
#9435=CARTESIAN_POINT('Ctrl Pts',(4.38286813413549,1.86598787435336,2.03085801275357));
#9436=CARTESIAN_POINT('Ctrl Pts',(4.46906499874804,1.89658829808944,2.0255953723878));
#9437=CARTESIAN_POINT('Ctrl Pts',(4.68053928028881,1.95567337128066,2.01282934090382));
#9438=CARTESIAN_POINT('Ctrl Pts',(4.80704042443649,1.97818409794303,2.00529278787818));
#9439=CARTESIAN_POINT('Ctrl Pts',(4.95099119604566,1.98969563311818,1.99633749199456));
#9440=CARTESIAN_POINT('Ctrl Pts',(4.9671796843881,1.99079160579118,1.99532548432424));
#9441=CARTESIAN_POINT('Ctrl Pts',(4.99358439491918,1.99225586059443,1.99366601371448));
#9442=CARTESIAN_POINT('Ctrl Pts',(5.00379345406848,1.99274332303448,1.9930222590483));
#9443=CARTESIAN_POINT('Ctrl Pts',(5.02205392319621,1.99347461586095,1.99186678946396));
#9444=CARTESIAN_POINT('Ctrl Pts',(5.03010396839057,1.9937481769985,1.99135601181253));
#9445=CARTESIAN_POINT('Ctrl Pts',(5.04716569491351,1.994224541048,1.99027039036127));
#9446=CARTESIAN_POINT('Ctrl Pts',(5.0561775127827,1.99441503003834,1.98969517450829));
#9447=CARTESIAN_POINT('Ctrl Pts',(5.08029634194139,1.99476131965319,1.98815072127568));
#9448=CARTESIAN_POINT('Ctrl Pts',(5.09540411274227,1.99480658153842,1.98717807087926));
#9449=CARTESIAN_POINT('Ctrl Pts',(5.1710639023163,1.99417376521607,1.98227985532387));
#9450=CARTESIAN_POINT('Ctrl Pts',(5.23155677862222,1.99091029114466,1.9782749306638));
#9451=CARTESIAN_POINT('Ctrl Pts',(5.41865194796816,1.97224928255046,1.96560703263229));
#9452=CARTESIAN_POINT('Ctrl Pts',(5.54398486227364,1.94746750731485,1.95669629285439));
#9453=CARTESIAN_POINT('Ctrl Pts',(5.75953130068192,1.88291845464412,1.94103254837983));
#9454=CARTESIAN_POINT('Ctrl Pts',(5.85081543380803,1.84811177632074,1.93429255838266));
#9455=CARTESIAN_POINT('Ctrl Pts',(5.94907212931743,1.80213832006741,1.9271630749843));
#9456=CARTESIAN_POINT('Ctrl Pts',(5.95891196845178,1.79743560916145,1.92645062905898));
#9457=CARTESIAN_POINT('Ctrl Pts',(5.97376597049668,1.79018626352909,1.92537801233651));
#9458=CARTESIAN_POINT('Ctrl Pts',(5.9788085611389,1.7876988252523,1.9250143901954));
#9459=CARTESIAN_POINT('Ctrl Pts',(5.98786477122631,1.7831838163046,1.92436234884548));
#9460=CARTESIAN_POINT('Ctrl Pts',(5.99188209244253,1.78116397686074,1.92407346827394));
#9461=CARTESIAN_POINT('Ctrl Pts',(5.99591029478403,1.77912157331222,1.92378417215569));
#9462=CARTESIAN_POINT('Ctrl Pts',(5.99592790994126,1.77911264163964,1.92378290708299));
#9463=CARTESIAN_POINT('Ctrl Pts',(5.99596290533334,1.77909489675728,1.92378039382278));
#9464=CARTESIAN_POINT('Ctrl Pts',(5.99598028551632,1.77908608358249,1.92377914563881));
#9465=CARTESIAN_POINT('Ctrl Pts',(5.99601481435387,1.7790685740007,1.92377666591178));
#9466=CARTESIAN_POINT('Ctrl Pts',(5.99603196306253,1.77905987757471,1.92377543436464));
#9467=CARTESIAN_POINT('Ctrl Pts',(5.99606603252794,1.77904259970207,1.92377298765389));
#9468=CARTESIAN_POINT('Ctrl Pts',(5.99608295328133,1.77903401826534,1.92377177249034));
#9469=CARTESIAN_POINT('Ctrl Pts',(5.99611657020711,1.77901696868618,1.92376935830415));
#9470=CARTESIAN_POINT('Ctrl Pts',(5.99613326639525,1.77900850054376,1.92376815928021));
#9471=CARTESIAN_POINT('Ctrl Pts',(5.996166437788,1.77899167575248,1.92376577711439));
#9472=CARTESIAN_POINT('Ctrl Pts',(5.99618291289591,1.77898331916044,1.92376459397928));
#9473=CARTESIAN_POINT('Ctrl Pts',(5.99621564508729,1.77896671599219,1.92376224337815));
#9474=CARTESIAN_POINT('Ctrl Pts',(5.9962319022911,1.7789584693625,1.92376107590331));
#9475=CARTESIAN_POINT('Ctrl Pts',(5.99626420221967,1.77894208434307,1.92375875636761));
#9476=CARTESIAN_POINT('Ctrl Pts',(5.99628024485766,1.77893394600468,1.92375760431284));
#9477=CARTESIAN_POINT('Ctrl Pts',(5.99631211889415,1.77891777594637,1.92375531538416));
#9478=CARTESIAN_POINT('Ctrl Pts',(5.99632795023058,1.77890974426506,1.92375417851457));
#9479=CARTESIAN_POINT('Ctrl Pts',(5.99635940445583,1.7788937861258,1.92375191975534));
#9480=CARTESIAN_POINT('Ctrl Pts',(5.99637502748337,1.77888585960443,1.92375079785558));
#9481=CARTESIAN_POINT('Ctrl Pts',(5.9964060686142,1.77887011001812,1.92374856878256));
#9482=CARTESIAN_POINT('Ctrl Pts',(5.9964214865825,1.77886228702843,1.92374746161885));
#9483=CARTESIAN_POINT('Ctrl Pts',(5.9964521204165,1.77884674309396,1.92374526181487));
#9484=CARTESIAN_POINT('Ctrl Pts',(5.99646733632971,1.77883902213162,1.92374416917106));
#9485=CARTESIAN_POINT('Ctrl Pts',(5.99649756890053,1.77882368082681,1.92374199820201));
#9486=CARTESIAN_POINT('Ctrl Pts',(5.99651258566599,1.77881606043598,1.9237409198689));
#9487=CARTESIAN_POINT('Ctrl Pts',(5.99654242319735,1.77880091864089,1.92373877728707));
#9488=CARTESIAN_POINT('Ctrl Pts',(5.99655724387355,1.77879339728835,1.92373771304465));
#9489=CARTESIAN_POINT('Ctrl Pts',(5.99658669190428,1.77877845222938,1.9237355984515));
#9490=CARTESIAN_POINT('Ctrl Pts',(5.9966013193187,1.77877102849857,1.92373454809635));
#9491=CARTESIAN_POINT('Ctrl Pts',(5.99663038372448,1.77875627722994,1.92373246106921));
#9492=CARTESIAN_POINT('Ctrl Pts',(5.99664482072874,1.77874894969143,1.92373142439618));
#9493=CARTESIAN_POINT('Ctrl Pts',(5.99667350712362,1.77873438939899,1.92372936453119));
#9494=CARTESIAN_POINT('Ctrl Pts',(5.99668775650225,1.77872715665685,1.92372834133997));
#9495=CARTESIAN_POINT('Ctrl Pts',(5.99671607052577,1.77871278451236,1.92372630823145));
#9496=CARTESIAN_POINT('Ctrl Pts',(5.99673013509837,1.77870564515225,1.92372529831922));
#9497=CARTESIAN_POINT('Ctrl Pts',(5.99675808198086,1.77869145853409,1.9237232915909));
#9498=CARTESIAN_POINT('Ctrl Pts',(5.99677196436856,1.77868441124192,1.92372229476911));
#9499=CARTESIAN_POINT('Ctrl Pts',(5.99679954967086,1.77867040735962,1.92372031402101));
#9500=CARTESIAN_POINT('Ctrl Pts',(5.99681325256722,1.77866345078398,1.9237193300959));
#9501=CARTESIAN_POINT('Ctrl Pts',(5.99684048147304,1.77864962703747,1.92371737495515));
#9502=CARTESIAN_POINT('Ctrl Pts',(5.99685400747479,1.77864275987561,1.92371640373995));
#9503=CARTESIAN_POINT('Ctrl Pts',(5.9968808852602,1.77862911361693,1.92371447382707));
#9504=CARTESIAN_POINT('Ctrl Pts',(5.99689423699637,1.77862233454918,1.92371351513269));
#9505=CARTESIAN_POINT('Ctrl Pts',(5.99692076856352,1.77860886331922,1.92371161009505));
#9506=CARTESIAN_POINT('Ctrl Pts',(5.99693394848435,1.77860217111622,1.92371066374524));
#9507=CARTESIAN_POINT('Ctrl Pts',(5.99696013901644,1.77858887231224,1.92370878321007));
#9508=CARTESIAN_POINT('Ctrl Pts',(5.99697314962433,1.77858226571767,1.92370784902485));
#9509=CARTESIAN_POINT('Ctrl Pts',(5.99699900403606,1.77856913687232,1.92370599263868));
#9510=CARTESIAN_POINT('Ctrl Pts',(5.99701184779509,1.77856261464887,1.92370507044084));
#9511=CARTESIAN_POINT('Ctrl Pts',(5.99703737090359,1.77854965334346,1.92370323785721));
#9512=CARTESIAN_POINT('Ctrl Pts',(5.99705005022729,1.77854321427903,1.92370232747318));
#9513=CARTESIAN_POINT('Ctrl Pts',(5.99707609729567,1.77852998619227,1.92370045728329));
#9514=CARTESIAN_POINT('Ctrl Pts',(5.99708946505468,1.77852319714364,1.92369949747681));
#9515=CARTESIAN_POINT('Ctrl Pts',(6.00199921851898,1.77602962392392,1.92334697811698));
#9516=CARTESIAN_POINT('Ctrl Pts',(6.00688538425036,1.7735225946533,1.92299668092783));
#9517=CARTESIAN_POINT('Ctrl Pts',(6.02129243550442,1.76605519918921,1.92196519684877));
#9518=CARTESIAN_POINT('Ctrl Pts',(6.03078387972458,1.76103802376924,1.92128743908224));
#9519=CARTESIAN_POINT('Ctrl Pts',(6.05257600510387,1.74929264589705,1.91973439398466));
#9520=CARTESIAN_POINT('Ctrl Pts',(6.06484731532463,1.7425108294251,1.91886214259767));
#9521=CARTESIAN_POINT('Ctrl Pts',(6.20487975197366,1.66318229925407,1.90892301870525));
#9522=CARTESIAN_POINT('Ctrl Pts',(6.32433823506054,1.57685362073657,1.90055841904611));
#9523=CARTESIAN_POINT('Ctrl Pts',(6.52195257802618,1.39778997876207,1.88502988379646));
#9524=CARTESIAN_POINT('Ctrl Pts',(6.6032363949858,1.30959431306031,1.87796376276932));
#9525=CARTESIAN_POINT('Ctrl Pts',(6.68604408267547,1.20172312826808,1.86953146912589));
#9526=CARTESIAN_POINT('Ctrl Pts',(6.69580987867472,1.18867344144245,1.86851494178726));
#9527=CARTESIAN_POINT('Ctrl Pts',(6.71145056117932,1.16723048110878,1.86684953568607));
#9528=CARTESIAN_POINT('Ctrl Pts',(6.71742275809633,1.15890887976216,1.86620441025367));
#9529=CARTESIAN_POINT('Ctrl Pts',(6.72797773045962,1.14395995458449,1.86504742410944));
#9530=CARTESIAN_POINT('Ctrl Pts',(6.73258497235119,1.1373501193316,1.8645365103754));
#9531=CARTESIAN_POINT('Ctrl Pts',(6.7422540649355,1.12329751257589,1.86345159632207));
#9532=CARTESIAN_POINT('Ctrl Pts',(6.74730582398839,1.11584804789945,1.86287723032537));
#9533=CARTESIAN_POINT('Ctrl Pts',(6.76066844719456,1.0958531497276,1.86133746569626));
#9534=CARTESIAN_POINT('Ctrl Pts',(6.76888792355924,1.08324762647418,1.86036869013031));
#9535=CARTESIAN_POINT('Ctrl Pts',(6.80904631599262,1.0201099637075,1.85552495940285));
#9536=CARTESIAN_POINT('Ctrl Pts',(6.83884210141049,0.968257562903548,1.85157276357886));
#9537=CARTESIAN_POINT('Ctrl Pts',(6.93899042394852,0.774293234319279,1.83687300423142));
#9538=CARTESIAN_POINT('Ctrl Pts',(6.99466232358782,0.625277353532774,1.82568225382217));
#9539=CARTESIAN_POINT('Ctrl Pts',(7.04087087708038,0.435229225678174,1.8121777195781));
#9540=CARTESIAN_POINT('Ctrl Pts',(7.04862847668504,0.39894334917576,1.80963558122238));
#9541=CARTESIAN_POINT('Ctrl Pts',(7.06154546629564,0.329039949266209,1.80483084415302));
#9542=CARTESIAN_POINT('Ctrl Pts',(7.066866353894,0.295464524088075,1.80256344834977));
#9543=CARTESIAN_POINT('Ctrl Pts',(7.0724832565604,0.253032086363658,1.79976177479462));
#9544=CARTESIAN_POINT('Ctrl Pts',(7.07358169352563,0.244289130020815,1.79918790561487));
#9545=CARTESIAN_POINT('Ctrl Pts',(7.07523088605998,0.230420036124329,1.7982832545103));
#9546=CARTESIAN_POINT('Ctrl Pts',(7.07581975052471,0.225298671204406,1.79795042589789));
#9547=CARTESIAN_POINT('Ctrl Pts',(7.0768764662282,0.215783495205807,1.79733440074816));
#9548=CARTESIAN_POINT('Ctrl Pts',(7.07734956854153,0.211390451495288,1.79705092671119));
#9549=CARTESIAN_POINT('Ctrl Pts',(7.07826738932372,0.202593464129223,1.79648511417043));
#9550=CARTESIAN_POINT('Ctrl Pts',(7.07871204618241,0.198189618732565,1.79620278115165));
#9551=CARTESIAN_POINT('Ctrl Pts',(7.07970451006276,0.188021852125648,1.79555296146577));
#9552=CARTESIAN_POINT('Ctrl Pts',(7.08024189093331,0.182256920403751,1.79518603892067));
#9553=CARTESIAN_POINT('Ctrl Pts',(7.08156992230612,0.167305893814251,1.79423817719713));
#9554=CARTESIAN_POINT('Ctrl Pts',(7.08232200875522,0.158116396954387,1.7936592317831));
#9555=CARTESIAN_POINT('Ctrl Pts',(7.08668811633936,0.0997972873341222,1.790006340589));
#9556=CARTESIAN_POINT('Ctrl Pts',(7.08854511044351,0.0505497621316073,1.78701713277168));
#9557=CARTESIAN_POINT('Ctrl Pts',(7.08857674428943,0.0012807565402712,1.78407775478297));
#9558=CARTESIAN_POINT('Ctrl Pts',(7.08857697543068,0.000847466486718941,
1.62559580923438));
#9559=CARTESIAN_POINT('Ctrl Pts',(7.0885186478675,0.13813772867541,1.6346093415605));
#9560=CARTESIAN_POINT('Ctrl Pts',(7.0742870217937,0.275032186647476,1.64406239390923));
#9561=CARTESIAN_POINT('Ctrl Pts',(7.02136448036863,0.527429007289867,1.66203452124581));
#9562=CARTESIAN_POINT('Ctrl Pts',(6.98594482700694,0.643022062967079,1.67048117357389));
#9563=CARTESIAN_POINT('Ctrl Pts',(6.9342345859718,0.769535207729763,1.67953767511746));
#9564=CARTESIAN_POINT('Ctrl Pts',(6.92799797735193,0.784283992593526,1.6805901674866));
#9565=CARTESIAN_POINT('Ctrl Pts',(6.919177355224,0.80446275310561,1.68202402410278));
#9566=CARTESIAN_POINT('Ctrl Pts',(6.91674558763128,0.809958063607057,1.68241387742721));
#9567=CARTESIAN_POINT('Ctrl Pts',(6.91254014766623,0.819346639764221,1.68307874378594));
#9568=CARTESIAN_POINT('Ctrl Pts',(6.91077873336726,0.823245302745461,1.68335448156896));
#9569=CARTESIAN_POINT('Ctrl Pts',(6.90708649128147,0.831348028823863,1.68392677710576));
#9570=CARTESIAN_POINT('Ctrl Pts',(6.90515356693689,0.835551072967431,1.68422319329436));
#9571=CARTESIAN_POINT('Ctrl Pts',(6.9004273923886,0.84573442154125,1.68494036848763));
#9572=CARTESIAN_POINT('Ctrl Pts',(6.89761901556641,0.851707729337802,1.68536021027999));
#9573=CARTESIAN_POINT('Ctrl Pts',(6.88757187304332,0.87280500605721,1.68684047699931));
#9574=CARTESIAN_POINT('Ctrl Pts',(6.88017189635716,0.887852015034895,1.68789151483874));
#9575=CARTESIAN_POINT('Ctrl Pts',(6.86139847977402,0.924840444295633,1.69046780629416));
#9576=CARTESIAN_POINT('Ctrl Pts',(6.84980512988548,0.94666768205827,1.69198160424515));
#9577=CARTESIAN_POINT('Ctrl Pts',(6.79950021875832,1.03727298462176,1.6982614381187));
#9578=CARTESIAN_POINT('Ctrl Pts',(6.75712774792099,1.10394243196616,1.70287436838431));
#9579=CARTESIAN_POINT('Ctrl Pts',(6.61786958130527,1.29675573459564,1.7167033108207));
#9580=CARTESIAN_POINT('Ctrl Pts',(6.50977763753097,1.41398692410837,1.7258447971311));
#9581=CARTESIAN_POINT('Ctrl Pts',(6.37244731286415,1.53121767622822,1.73696642571239));
#9582=CARTESIAN_POINT('Ctrl Pts',(6.35573939200201,1.54501602901815,1.73831117597603));
#9583=CARTESIAN_POINT('Ctrl Pts',(6.3296140732491,1.56588530796427,1.74040318463983));
#9584=CARTESIAN_POINT('Ctrl Pts',(6.32035296875346,1.57314987326505,1.74114275003695));
#9585=CARTESIAN_POINT('Ctrl Pts',(6.30451665109693,1.58534730035983,1.74240426414843));
#9586=CARTESIAN_POINT('Ctrl Pts',(6.29797417678056,1.59032231493196,1.7429245419122));
#9587=CARTESIAN_POINT('Ctrl Pts',(6.28467472438383,1.60030633777818,1.74398045916568));
#9588=CARTESIAN_POINT('Ctrl Pts',(6.27791644277611,1.60531332245671,1.74451616273635));
#9589=CARTESIAN_POINT('Ctrl Pts',(6.26118376939706,1.61754684860185,1.74584047196962));
#9590=CARTESIAN_POINT('Ctrl Pts',(6.25117382988796,1.62472395670157,1.74663095544629));
#9591=CARTESIAN_POINT('Ctrl Pts',(6.21365723330576,1.65110065833184,1.74958760390165));
#9592=CARTESIAN_POINT('Ctrl Pts',(6.18573541055629,1.66969725532199,1.75177628304859));
#9593=CARTESIAN_POINT('Ctrl Pts',(6.11457383764612,1.71454408695528,1.7573285197755));
#9594=CARTESIAN_POINT('Ctrl Pts',(6.0707815794354,1.73986912475829,1.76072268879818));
#9595=CARTESIAN_POINT('Ctrl Pts',(5.92261414724874,1.81819574979078,1.77212382054799));
#9596=CARTESIAN_POINT('Ctrl Pts',(5.81454439380532,1.86367547879841,1.78032425845484));
#9597=CARTESIAN_POINT('Ctrl Pts',(5.61737875461597,1.92692241665534,1.79471975571545));
#9598=CARTESIAN_POINT('Ctrl Pts',(5.52985919385639,1.94859337517318,1.80091974923904));
#9599=CARTESIAN_POINT('Ctrl Pts',(5.4303822768349,1.96618364594338,1.80755949173854));
#9600=CARTESIAN_POINT('Ctrl Pts',(5.41958310089061,1.968001665715,1.80827493851534));
#9601=CARTESIAN_POINT('Ctrl Pts',(5.40320753263651,1.97061997041465,1.80935116098224));
#9602=CARTESIAN_POINT('Ctrl Pts',(5.39764202753576,1.97148568621826,1.80971542188362));
#9603=CARTESIAN_POINT('Ctrl Pts',(5.38762647144156,1.97300018924479,1.81036813128623));
#9604=CARTESIAN_POINT('Ctrl Pts',(5.38317784757979,1.9736575090386,1.81065704564296));
#9605=CARTESIAN_POINT('Ctrl Pts',(5.37339936030238,1.97506858575359,1.81128990674961));
#9606=CARTESIAN_POINT('Ctrl Pts',(5.36806866058057,1.9758158149631,1.81163348650117));
#9607=CARTESIAN_POINT('Ctrl Pts',(5.35272874880679,1.97790280455986,1.81261827241101));
#9608=CARTESIAN_POINT('Ctrl Pts',(5.34271213002741,1.97918817166451,1.81325652390456));
#9609=CARTESIAN_POINT('Ctrl Pts',(5.26998901477252,1.98795941837045,1.8178584752704));
#9610=CARTESIAN_POINT('Ctrl Pts',(5.20696135822694,1.99254059429888,1.82167541324663));
#9611=CARTESIAN_POINT('Ctrl Pts',(5.01315008934833,1.99739909857102,1.8331732542045));
#9612=CARTESIAN_POINT('Ctrl Pts',(4.88247521016737,1.98782419847057,1.84061123969016));
#9613=CARTESIAN_POINT('Ctrl Pts',(4.66583816701276,1.95033300652042,1.85354398893336));
#9614=CARTESIAN_POINT('Ctrl Pts',(4.57913208347251,1.92926397660002,1.85888463572897));
#9615=CARTESIAN_POINT('Ctrl Pts',(4.47919163793529,1.89776082036726,1.86538783022986));
#9616=CARTESIAN_POINT('Ctrl Pts',(4.46430778045187,1.89287566560678,1.86636544765753));
#9617=CARTESIAN_POINT('Ctrl Pts',(4.43997105879876,1.88456912625687,1.86797970652299));
#9618=CARTESIAN_POINT('Ctrl Pts',(4.43048360992003,1.88125062696164,1.86861297452493));
#9619=CARTESIAN_POINT('Ctrl Pts',(4.4134545918659,1.87514942076045,1.86975695979694));
#9620=CARTESIAN_POINT('Ctrl Pts',(4.40590394964709,1.87239254305697,1.87026681402807));
#9621=CARTESIAN_POINT('Ctrl Pts',(4.38982216108017,1.86641038127407,1.87135841618666));
#9622=CARTESIAN_POINT('Ctrl Pts',(4.38129608390681,1.86317208302679,1.87194058748928));
#9623=CARTESIAN_POINT('Ctrl Pts',(4.35825305961791,1.85423878810684,1.87352348600471));
#9624=CARTESIAN_POINT('Ctrl Pts',(4.34378044088254,1.84843194002899,1.87452792809919));
#9625=CARTESIAN_POINT('Ctrl Pts',(4.26708695076379,1.81661121241874,1.87990681093444));
#9626=CARTESIAN_POINT('Ctrl Pts',(4.20615370851447,1.78762685080172,1.88438068049406));
#9627=CARTESIAN_POINT('Ctrl Pts',(4.00331996138289,1.67821397657109,1.89997570611706));
#9628=CARTESIAN_POINT('Ctrl Pts',(3.86986483666516,1.58351324221346,1.91152928418664));
#9629=CARTESIAN_POINT('Ctrl Pts',(3.70846184219961,1.43626865884864,1.92652310852278));
#9630=CARTESIAN_POINT('Ctrl Pts',(3.66905407985949,1.39718559945625,1.93027437348577));
#9631=CARTESIAN_POINT('Ctrl Pts',(3.62500104265978,1.3496902802352,1.93452624992127));
#9632=CARTESIAN_POINT('Ctrl Pts',(3.61872611184866,1.34282944609183,1.93513334110161));
#9633=CARTESIAN_POINT('Ctrl Pts',(3.60863726499821,1.33164252140809,1.93611143232783));
#9634=CARTESIAN_POINT('Ctrl Pts',(3.60479382140584,1.32734341737144,1.93648452613418));
#9635=CARTESIAN_POINT('Ctrl Pts',(3.5979808863196,1.31965593960071,1.93714664064215));
#9636=CARTESIAN_POINT('Ctrl Pts',(3.59500418097798,1.31627411748113,1.93743618897301));
#9637=CARTESIAN_POINT('Ctrl Pts',(3.58856535921404,1.30890883548465,1.93806305069477));
#9638=CARTESIAN_POINT('Ctrl Pts',(3.58510758733448,1.3049217145677,1.93840004752316));
#9639=CARTESIAN_POINT('Ctrl Pts',(3.57540102253982,1.2936390191853,1.93934723192615));
#9640=CARTESIAN_POINT('Ctrl Pts',(3.56918894500103,1.28631184750864,1.93995480553468));
#9641=CARTESIAN_POINT('Ctrl Pts',(3.53026935687444,1.23972795543907,1.94377229797163));
#9642=CARTESIAN_POINT('Ctrl Pts',(3.49902441645861,1.19926794103641,1.94688661808404));
#9643=CARTESIAN_POINT('Ctrl Pts',(3.38111956289245,1.03381886743734,1.95904223294462));
#9644=CARTESIAN_POINT('Ctrl Pts',(3.30731812864984,0.900300008321492,1.96763354781027));
#9645=CARTESIAN_POINT('Ctrl Pts',(3.21843452097759,0.684500953130051,1.98141284969103));
#9646=CARTESIAN_POINT('Ctrl Pts',(3.19209697690137,0.607502350096773,1.98630303843298));
#9647=CARTESIAN_POINT('Ctrl Pts',(3.16645679492729,0.514302584381907,1.99230445155953));
#9648=CARTESIAN_POINT('Ctrl Pts',(3.16255247547667,0.499441432852979,1.99326367682759));
#9649=CARTESIAN_POINT('Ctrl Pts',(3.15640103345556,0.474875542138074,1.99485372265693));
#9650=CARTESIAN_POINT('Ctrl Pts',(3.15405418294834,0.465196268351635,1.995481343078));
#9651=CARTESIAN_POINT('Ctrl Pts',(3.14994612472778,0.447681353724132,1.99661923856131));
#9652=CARTESIAN_POINT('Ctrl Pts',(3.14815955378462,0.439851835090765,1.99712869056361));
#9653=CARTESIAN_POINT('Ctrl Pts',(3.14443145456124,0.423046448523216,1.99822397213832));
#9654=CARTESIAN_POINT('Ctrl Pts',(3.14250454089642,0.414067561573615,1.99881025480113));
#9655=CARTESIAN_POINT('Ctrl Pts',(3.13741443595816,0.389524182950732,2.00041595769839));
#9656=CARTESIAN_POINT('Ctrl Pts',(3.13437508182302,0.373934974472855,2.00143927698293));
#9657=CARTESIAN_POINT('Ctrl Pts',(3.11858288505755,0.287448481973071,2.00713669966753));
#9658=CARTESIAN_POINT('Ctrl Pts',(3.10949294634671,0.215944847970046,2.01192491895846));
#9659=CARTESIAN_POINT('Ctrl Pts',(3.0927320733747,-0.0154454677935332,2.02766691509111));
#9660=CARTESIAN_POINT('Ctrl Pts',(3.10041094744031,-0.175793402475635,2.03900417881268));
#9661=CARTESIAN_POINT('Ctrl Pts',(3.13610531763832,-0.386290889499241,2.05364054535397));
#9662=CARTESIAN_POINT('Ctrl Pts',(3.14718200608279,-0.438713127306731,2.05725798109177));
#9663=CARTESIAN_POINT('Ctrl Pts',(3.16262315696911,-0.49956342259038,2.06137780864298));
#9664=CARTESIAN_POINT('Ctrl Pts',(3.16495186141941,-0.508480682786174,2.06197951216228));
#9665=CARTESIAN_POINT('Ctrl Pts',(3.16883168362759,-0.522927306642616,2.06295065616983));
#9666=CARTESIAN_POINT('Ctrl Pts',(3.17034499137608,-0.528466556222705,2.0633221435079));
#9667=CARTESIAN_POINT('Ctrl Pts',(3.17308778898029,-0.53833830360861,2.06398252579143));
#9668=CARTESIAN_POINT('Ctrl Pts',(3.17430804920743,-0.542673239748834,2.0642719371742));
#9669=CARTESIAN_POINT('Ctrl Pts',(3.1769951491051,-0.552096607311319,2.06489979234198));
#9670=CARTESIAN_POINT('Ctrl Pts',(3.17846757229804,-0.557183338896319,2.0652379108631));
#9671=CARTESIAN_POINT('Ctrl Pts',(3.18269133641752,-0.571560427272183,2.06619146447219));
#9672=CARTESIAN_POINT('Ctrl Pts',(3.18549017834018,-0.580836837302783,2.06680422925057));
#9673=CARTESIAN_POINT('Ctrl Pts',(3.20399680543207,-0.640596656856699,2.07073784496737));
#9674=CARTESIAN_POINT('Ctrl Pts',(3.22164029738127,-0.690463806925515,2.07395624778665));
#9675=CARTESIAN_POINT('Ctrl Pts',(3.30339792252517,-0.89526053767156,2.08713139326545));
#9676=CARTESIAN_POINT('Ctrl Pts',(3.38492692698709,-1.04249459169457,2.09655560371181));
#9677=CARTESIAN_POINT('Ctrl Pts',(3.52262843973057,-1.23071542513694,2.11044626762472));
#9678=CARTESIAN_POINT('Ctrl Pts',(3.56392080412243,-1.28168291693147,2.11442014690451));
#9679=CARTESIAN_POINT('Ctrl Pts',(3.61826224435822,-1.34238189730793,2.11948455624988));
#9680=CARTESIAN_POINT('Ctrl Pts',(3.62902149384696,-1.35411421815771,2.12047976115093));
#9681=CARTESIAN_POINT('Ctrl Pts',(3.64627610461419,-1.3724830455099,2.12206475075751));
#9682=CARTESIAN_POINT('Ctrl Pts',(3.65267951429091,-1.37920528808382,2.12265062168663));
#9683=CARTESIAN_POINT('Ctrl Pts',(3.6647029454159,-1.39165222217593,2.12374650358928));
#9684=CARTESIAN_POINT('Ctrl Pts',(3.67031104633254,-1.3973882063366,2.12425599256076));
#9685=CARTESIAN_POINT('Ctrl Pts',(3.6828647725479,-1.41007420336093,2.12539290029009));
#9686=CARTESIAN_POINT('Ctrl Pts',(3.68982742128975,-1.41700700271386,2.12602106041877));
#9687=CARTESIAN_POINT('Ctrl Pts',(3.71033930501654,-1.4371313523716,2.12786484534362));
#9688=CARTESIAN_POINT('Ctrl Pts',(3.72402494247374,-1.45018171719798,2.12908652942289));
#9689=CARTESIAN_POINT('Ctrl Pts',(3.84308779334311,-1.56052855554241,2.13964612411791));
#9690=CARTESIAN_POINT('Ctrl Pts',(3.95846958813204,-1.64637379662709,2.14946996585542));
#9691=CARTESIAN_POINT('Ctrl Pts',(4.19245013777418,-1.78408608232134,2.16837758074954));
#9692=CARTESIAN_POINT('Ctrl Pts',(4.308883236307,-1.83829054360325,2.17737319557314));
#9693=CARTESIAN_POINT('Ctrl Pts',(4.44454878346505,-1.88618993949204,2.18690315290051));
#9694=CARTESIAN_POINT('Ctrl Pts',(4.459440288013,-1.89125044119926,2.18793661198135));
#9695=CARTESIAN_POINT('Ctrl Pts',(4.48006764284195,-1.89798906508824,2.18934932696208));
#9696=CARTESIAN_POINT('Ctrl Pts',(4.48575304725337,-1.89981817857702,2.1897367476822));
#9697=CARTESIAN_POINT('Ctrl Pts',(4.49551560608305,-1.90291068365749,2.19039854260204));
#9698=CARTESIAN_POINT('Ctrl Pts',(4.49958871743466,-1.90418656116014,2.19067362731709));
#9699=CARTESIAN_POINT('Ctrl Pts',(4.5080926791622,-1.90682043245434,2.19124576978082));
#9700=CARTESIAN_POINT('Ctrl Pts',(4.51252420228966,-1.90817607036028,2.19154267977607));
#9701=CARTESIAN_POINT('Ctrl Pts',(4.52331927003924,-1.91143727077997,2.19226301416058));
#9702=CARTESIAN_POINT('Ctrl Pts',(4.52968776085435,-1.91332653614393,2.1926855014915));
#9703=CARTESIAN_POINT('Ctrl Pts',(4.55242563418988,-1.91994851602255,2.19418553827451));
#9704=CARTESIAN_POINT('Ctrl Pts',(4.56884661151151,-1.92450341268009,2.1952533652806));
#9705=CARTESIAN_POINT('Ctrl Pts',(4.60973921928892,-1.93528394172807,2.19787887672789));
#9706=CARTESIAN_POINT('Ctrl Pts',(4.63427502756244,-1.94125655864457,2.19942453130822));
#9707=CARTESIAN_POINT('Ctrl Pts',(4.73883285779753,-1.96461487400764,2.205911347083));
#9708=CARTESIAN_POINT('Ctrl Pts',(4.81977685118149,-1.97753155351539,2.21068883075821));
#9709=CARTESIAN_POINT('Ctrl Pts',(5.0551081552201,-2.0003526178119,2.22442787810779));
#9710=CARTESIAN_POINT('Ctrl Pts',(5.21011862229985,-1.99734324320496,2.23333647179194));
#9711=CARTESIAN_POINT('Ctrl Pts',(5.38738925048083,-1.97318112629982,2.24435253024693));
#9712=CARTESIAN_POINT('Ctrl Pts',(5.41149302194494,-1.96944428143835,2.24586710710607));
#9713=CARTESIAN_POINT('Ctrl Pts',(5.44516517591006,-1.96358981742938,2.24800891909488));
#9714=CARTESIAN_POINT('Ctrl Pts',(5.45479630849116,-1.96184215492393,2.24862452705035));
#9715=CARTESIAN_POINT('Ctrl Pts',(5.47245683009992,-1.95850303310291,2.24975903973385));
#9716=CARTESIAN_POINT('Ctrl Pts',(5.48049007194776,-1.95693289281094,2.25027726067193));
#9717=CARTESIAN_POINT('Ctrl Pts',(5.4968009064896,-1.95364049941748,2.25133397254712));
#9718=CARTESIAN_POINT('Ctrl Pts',(5.50507766032501,-1.95191497346157,2.25187255784419));
#9719=CARTESIAN_POINT('Ctrl Pts',(5.52559180711936,-1.94750194406158,2.25321345953189));
#9720=CARTESIAN_POINT('Ctrl Pts',(5.537815188727,-1.94475169392781,2.25401775909664));
#9721=CARTESIAN_POINT('Ctrl Pts',(5.58417498885021,-1.93386093357323,2.25708899126347));
#9722=CARTESIAN_POINT('Ctrl Pts',(5.61811868939426,-1.92493564516567,2.25938076687164));
#9723=CARTESIAN_POINT('Ctrl Pts',(5.70347265611761,-1.90006731190146,2.26525703681875));
#9724=CARTESIAN_POINT('Ctrl Pts',(5.75450332920836,-1.88293111709827,2.26887691895692));
#9725=CARTESIAN_POINT('Ctrl Pts',(5.88853387054315,-1.83180378559905,2.27866089484497));
#9726=CARTESIAN_POINT('Ctrl Pts',(5.97003821806222,-1.79424526481523,2.28490700090815));
#9727=CARTESIAN_POINT('Ctrl Pts',(6.14002552152954,-1.70156050829027,2.29840405139285));
#9728=CARTESIAN_POINT('Ctrl Pts',(6.22729382693212,-1.64471783306534,2.30563689135189));
#9729=CARTESIAN_POINT('Ctrl Pts',(6.32267180790665,-1.57137982128751,2.31361265653518));
#9730=CARTESIAN_POINT('Ctrl Pts',(6.33548296428924,-1.56127659811982,2.31468534709351));
#9731=CARTESIAN_POINT('Ctrl Pts',(6.35339280035416,-1.54679251373565,2.31618524410383));
#9732=CARTESIAN_POINT('Ctrl Pts',(6.35859511472257,-1.5425416385639,2.31662095750045));
#9733=CARTESIAN_POINT('Ctrl Pts',(6.36732525972065,-1.5353342713384,2.31735205498524));
#9734=CARTESIAN_POINT('Ctrl Pts',(6.37086448313447,-1.53239172913787,2.31764841962198));
#9735=CARTESIAN_POINT('Ctrl Pts',(6.37801665717794,-1.52640335935194,2.31824721990174));
#9736=CARTESIAN_POINT('Ctrl Pts',(6.38162901330332,-1.52335690756484,2.3185496076446));
#9737=CARTESIAN_POINT('Ctrl Pts',(6.39057951192814,-1.51575398542618,2.31929882418905));
#9738=CARTESIAN_POINT('Ctrl Pts',(6.39590454750912,-1.51118208266376,2.31974454452688));
#9739=CARTESIAN_POINT('Ctrl Pts',(6.40757913073792,-1.5010511401374,2.32072198064465));
#9740=CARTESIAN_POINT('Ctrl Pts',(6.41391778924148,-1.49547968964539,2.321252833754));
#9741=CARTESIAN_POINT('Ctrl Pts',(6.43216608904699,-1.47923366526153,2.32278221880721));
#9742=CARTESIAN_POINT('Ctrl Pts',(6.44398323252484,-1.46845563078022,2.3237740050948));
#9743=CARTESIAN_POINT('Ctrl Pts',(6.48487055385752,-1.43025273929782,2.32721588207732));
#9744=CARTESIAN_POINT('Ctrl Pts',(6.51324659656555,-1.40209610231227,2.32962321679784));
#9745=CARTESIAN_POINT('Ctrl Pts',(6.59893849946325,-1.3117968006145,2.33702560471193));
#9746=CARTESIAN_POINT('Ctrl Pts',(6.65316530577674,-1.24685078707598,2.34190901336403));
#9747=CARTESIAN_POINT('Ctrl Pts',(6.77813788096399,-1.0762191893389,2.35419111760451));
#9748=CARTESIAN_POINT('Ctrl Pts',(6.84320402900208,-0.966863843601102,2.36160889506266));
#9749=CARTESIAN_POINT('Ctrl Pts',(6.90804051567228,-0.829622808686236,2.3709455829387));
#9750=CARTESIAN_POINT('Ctrl Pts',(6.91822659464173,-0.806976283978035,2.37248614457263));
#9751=CARTESIAN_POINT('Ctrl Pts',(6.93196805266002,-0.774834283425505,2.37467521152113));
#9752=CARTESIAN_POINT('Ctrl Pts',(6.93587811358629,-0.765492251020123,2.37531175571147));
#9753=CARTESIAN_POINT('Ctrl Pts',(6.94256794874434,-0.749160608642424,2.37642525400048));
#9754=CARTESIAN_POINT('Ctrl Pts',(6.94537966315552,-0.742184240624828,2.37690112584366));
#9755=CARTESIAN_POINT('Ctrl Pts',(6.95118552422492,-0.727540517259782,2.37790054457039));
#9756=CARTESIAN_POINT('Ctrl Pts',(6.95417179776423,-0.719870212470008,2.37842434380341));
#9757=CARTESIAN_POINT('Ctrl Pts',(6.96117797996114,-0.701539915944533,2.37967694818009));
#9758=CARTESIAN_POINT('Ctrl Pts',(6.9651541688795,-0.690863630097261,2.38040719054387));
#9759=CARTESIAN_POINT('Ctrl Pts',(6.97839082119528,-0.654369659089111,2.38290596348991));
#9760=CARTESIAN_POINT('Ctrl Pts',(6.98720981464392,-0.628396246926899,2.38468891210499));
#9761=CARTESIAN_POINT('Ctrl Pts',(7.00715082964822,-0.565430581908695,2.38902409113906));
#9762=CARTESIAN_POINT('Ctrl Pts',(7.01773902068331,-0.528282153670864,2.391592426768));
#9763=CARTESIAN_POINT('Ctrl Pts',(7.0679796882215,-0.330389330144033,2.4053291729097));
#9764=CARTESIAN_POINT('Ctrl Pts',(7.08857715545339,-0.165496138935671,2.41703857396203));
#9765=CARTESIAN_POINT('Ctrl Pts',(7.08857715545311,3.3222036233127E-12,
2.42843892255116));
#9766=CARTESIAN_POINT('Origin',(5.09382715545311,0.,-6.77268258743872));
#9767=CARTESIAN_POINT('',(7.08857715495384,-4.3655925271901E-5,3.38727862543405));
#9768=CARTESIAN_POINT('',(7.08857715545311,9.38914434820125E-11,3.22796126976449));
#9769=CARTESIAN_POINT('',(7.08857715545311,8.3550772080578E-14,-6.77268258743872));
#9770=CARTESIAN_POINT('Ctrl Pts',(7.08857715492703,-4.58127331705431E-5,
3.38727861359244));
#9771=CARTESIAN_POINT('Ctrl Pts',(7.08857709852051,-0.00250183082418328,
3.38712320877298));
#9772=CARTESIAN_POINT('Ctrl Pts',(7.08857250618887,-0.00495784000431415,
3.38696766332));
#9773=CARTESIAN_POINT('Ctrl Pts',(7.08854430155101,-0.0125464722495827,
3.38648661511498));
#9774=CARTESIAN_POINT('Ctrl Pts',(7.08850541512609,-0.0176789843406733,
3.38616063939049));
#9775=CARTESIAN_POINT('Ctrl Pts',(7.08834420420563,-0.031775294329847,3.38526361437851));
#9776=CARTESIAN_POINT('Ctrl Pts',(7.08818126235171,-0.0407384226304432,
3.38469130714592));
#9777=CARTESIAN_POINT('Ctrl Pts',(7.08758290455359,-0.0647465309243057,
3.38315303086674));
#9778=CARTESIAN_POINT('Ctrl Pts',(7.08703762158118,-0.0797879535402261,
3.38218366787627));
#9779=CARTESIAN_POINT('Ctrl Pts',(7.0836431288264,-0.151116869654046,3.37755920561389));
#9780=CARTESIAN_POINT('Ctrl Pts',(7.07857971239356,-0.207268340064208,3.37383612540531));
#9781=CARTESIAN_POINT('Ctrl Pts',(7.06586614929467,-0.302807314340294,3.36735657017158));
#9782=CARTESIAN_POINT('Ctrl Pts',(7.05939262223529,-0.342318791249575,3.36463416234251));
#9783=CARTESIAN_POINT('Ctrl Pts',(7.03693774861316,-0.457527846573419,3.35658050637764));
#9784=CARTESIAN_POINT('Ctrl Pts',(7.01773758018822,-0.532520541956035,3.35118747832221));
#9785=CARTESIAN_POINT('Ctrl Pts',(6.9704281920205,-0.680831781169107,3.34033565578518));
#9786=CARTESIAN_POINT('Ctrl Pts',(6.94224670858607,-0.753996021387809,3.33488630434343));
#9787=CARTESIAN_POINT('Ctrl Pts',(6.89965421953311,-0.847715453802603,3.32791491418379));
#9788=CARTESIAN_POINT('Ctrl Pts',(6.88906079774946,-0.869924801332104,3.32626381758821));
#9789=CARTESIAN_POINT('Ctrl Pts',(6.87058634868833,-0.906881251200297,3.32352458579133));
#9790=CARTESIAN_POINT('Ctrl Pts',(6.86292614477236,-0.921735127052531,3.32242588770936));
#9791=CARTESIAN_POINT('Ctrl Pts',(6.85198518917063,-0.942311701201185,3.32090888951387));
#9792=CARTESIAN_POINT('Ctrl Pts',(6.8488616202024,-0.948116577354574,3.320481488738));
#9793=CARTESIAN_POINT('Ctrl Pts',(6.84349781503736,-0.957967395749502,3.3197572878788));
#9794=CARTESIAN_POINT('Ctrl Pts',(6.84127219456565,-0.962021197932506,3.31945958339373));
#9795=CARTESIAN_POINT('Ctrl Pts',(6.83695957506552,-0.969811966024536,3.31888810504421));
#9796=CARTESIAN_POINT('Ctrl Pts',(6.83487463129223,-0.973549983031158,3.31861419937776));
#9797=CARTESIAN_POINT('Ctrl Pts',(6.82982980836454,-0.982526617793599,3.31795705875355));
#9798=CARTESIAN_POINT('Ctrl Pts',(6.82685820532529,-0.9877586486549,3.31757456135241));
#9799=CARTESIAN_POINT('Ctrl Pts',(6.8158634874209,-1.00691443052252,3.31617574350262));
#9800=CARTESIAN_POINT('Ctrl Pts',(6.80769562319996,-1.02075497187569,3.3151681812041));
#9801=CARTESIAN_POINT('Ctrl Pts',(6.73752655663979,-1.13644004665874,3.30675986233794));
#9802=CARTESIAN_POINT('Ctrl Pts',(6.66666750077952,-1.2326494397742,3.29984575532485));
#9803=CARTESIAN_POINT('Ctrl Pts',(6.51813664250263,-1.40048759101688,3.28683471699357));
#9804=CARTESIAN_POINT('Ctrl Pts',(6.442563525247,-1.47340803481055,3.28075881220056));
#9805=CARTESIAN_POINT('Ctrl Pts',(6.31953849316263,-1.57468390429232,3.27119210792828));
#9806=CARTESIAN_POINT('Ctrl Pts',(6.27606413925425,-1.60757973181704,3.26786738321616));
#9807=CARTESIAN_POINT('Ctrl Pts',(6.21929140428639,-1.64698861308956,3.26356259037007));
#9808=CARTESIAN_POINT('Ctrl Pts',(6.20719143362846,-1.65519220431611,3.26264720838283));
#9809=CARTESIAN_POINT('Ctrl Pts',(6.18867607129601,-1.66745044405147,3.26124913366752));
#9810=CARTESIAN_POINT('Ctrl Pts',(6.18232573140066,-1.6716028175036,3.26077009257741));
#9811=CARTESIAN_POINT('Ctrl Pts',(6.16935309855411,-1.67998012234839,3.25979235594394));
#9812=CARTESIAN_POINT('Ctrl Pts',(6.1627292362971,-1.68420236446147,3.2592935723595));
#9813=CARTESIAN_POINT('Ctrl Pts',(6.14813714804323,-1.69338302779993,3.25819566993454));
#9814=CARTESIAN_POINT('Ctrl Pts',(6.14015855464053,-1.69832453831343,3.25759594480215));
#9815=CARTESIAN_POINT('Ctrl Pts',(6.11772834641523,-1.71199854419326,3.2559113871023));
#9816=CARTESIAN_POINT('Ctrl Pts',(6.10320056127153,-1.72060395292479,3.2548219805004));
#9817=CARTESIAN_POINT('Ctrl Pts',(6.01538426104975,-1.7711262531708,3.24824511414507));
#9818=CARTESIAN_POINT('Ctrl Pts',(5.93961358814865,-1.80853467405239,3.24259917353566));
#9819=CARTESIAN_POINT('Ctrl Pts',(5.7241170264138,-1.8984171202113,3.22663956008988));
#9820=CARTESIAN_POINT('Ctrl Pts',(5.58053707097804,-1.9401963082779,3.21608165181089));
#9821=CARTESIAN_POINT('Ctrl Pts',(5.38367687892514,-1.97423064999869,3.20241605452096));
#9822=CARTESIAN_POINT('Ctrl Pts',(5.33338752889605,-1.98096221899896,3.19899844769956));
#9823=CARTESIAN_POINT('Ctrl Pts',(5.27334778529183,-1.98667859042588,3.19504538027708));
#9824=CARTESIAN_POINT('Ctrl Pts',(5.26379702098257,-1.98751848590658,3.19442036796973));
#9825=CARTESIAN_POINT('Ctrl Pts',(5.248983880856,-1.98871359510105,3.19345727616396));
#9826=CARTESIAN_POINT('Ctrl Pts',(5.24372568072868,-1.98911684082435,3.19311663695123));
#9827=CARTESIAN_POINT('Ctrl Pts',(5.23397198325351,-1.98982594502665,3.19248712201647));
#9828=CARTESIAN_POINT('Ctrl Pts',(5.22947707591475,-1.99013742338515,3.19219795052357));
#9829=CARTESIAN_POINT('Ctrl Pts',(5.21922143724784,-1.99081318894947,3.19154027227158));
#9830=CARTESIAN_POINT('Ctrl Pts',(5.21346015824319,-1.99116770409923,3.19117231121698));
#9831=CARTESIAN_POINT('Ctrl Pts',(5.19839681858278,-1.99202899839834,3.19021397959583));
#9832=CARTESIAN_POINT('Ctrl Pts',(5.18909247970869,-1.99249563883409,3.18962575503284));
#9833=CARTESIAN_POINT('Ctrl Pts',(5.12392116011475,-1.99530661507959,3.18552949407312));
#9834=CARTESIAN_POINT('Ctrl Pts',(5.06797502758653,-1.9953663918303,3.18213576354771));
#9835=CARTESIAN_POINT('Ctrl Pts',(4.84962392566178,-1.98641225485162,3.16911703124668));
#9836=CARTESIAN_POINT('Ctrl Pts',(4.68857411250159,-1.95990923518893,3.15995601572542));
#9837=CARTESIAN_POINT('Ctrl Pts',(4.46786717336476,-1.8951889669928,3.14626316818435));
#9838=CARTESIAN_POINT('Ctrl Pts',(4.40422149818246,-1.87296816013138,3.14217970589422));
#9839=CARTESIAN_POINT('Ctrl Pts',(4.32738670495393,-1.84169477419209,3.13701939913801));
#9840=CARTESIAN_POINT('Ctrl Pts',(4.31301685886521,-1.83564862230034,3.13604418342241));
#9841=CARTESIAN_POINT('Ctrl Pts',(4.2903559879828,-1.82579977272359,3.13448950528925));
#9842=CARTESIAN_POINT('Ctrl Pts',(4.28201744556825,-1.82210749340418,3.13391378715432));
#9843=CARTESIAN_POINT('Ctrl Pts',(4.26637710381656,-1.81505332962233,3.13282692284827));
#9844=CARTESIAN_POINT('Ctrl Pts',(4.2590697158949,-1.81170422291852,3.1323162216528));
#9845=CARTESIAN_POINT('Ctrl Pts',(4.24266997668752,-1.80406764586246,3.13116342234245));
#9846=CARTESIAN_POINT('Ctrl Pts',(4.23358944430854,-1.79975545228914,3.1305204837879));
#9847=CARTESIAN_POINT('Ctrl Pts',(4.2104388682996,-1.78854639967122,3.12886924426446));
#9848=CARTESIAN_POINT('Ctrl Pts',(4.19641700152983,-1.78155215532139,3.12785759782902));
#9849=CARTESIAN_POINT('Ctrl Pts',(4.10307121026518,-1.73360874231533,3.12104390016041));
#9850=CARTESIAN_POINT('Ctrl Pts',(4.02650162835934,-1.68754523144274,3.11506263111305));
#9851=CARTESIAN_POINT('Ctrl Pts',(3.84614174300541,-1.56184610571137,3.10000114368129));
#9852=CARTESIAN_POINT('Ctrl Pts',(3.74660107071103,-1.47684151982662,3.09079049378236));
#9853=CARTESIAN_POINT('Ctrl Pts',(3.61231596880704,-1.33721316506094,3.07744805969703));
#9854=CARTESIAN_POINT('Ctrl Pts',(3.57072795862261,-1.28964528920073,3.07316247995355));
#9855=CARTESIAN_POINT('Ctrl Pts',(3.52518485781038,-1.23227061743155,3.06835642938633));
#9856=CARTESIAN_POINT('Ctrl Pts',(3.51896668589212,-1.22431370334604,3.06769762919173));
#9857=CARTESIAN_POINT('Ctrl Pts',(3.50952695435974,-1.21204348445192,3.06669390928744));
#9858=CARTESIAN_POINT('Ctrl Pts',(3.50626209067189,-1.20776392648606,3.06634608441327));
#9859=CARTESIAN_POINT('Ctrl Pts',(3.50030144291197,-1.1998848230521,3.06570989861047));
#9860=CARTESIAN_POINT('Ctrl Pts',(3.49760051176691,-1.19628938300882,3.06542118910934));
#9861=CARTESIAN_POINT('Ctrl Pts',(3.49154399227421,-1.1881700010936,3.06477278318482));
#9862=CARTESIAN_POINT('Ctrl Pts',(3.48819539674085,-1.1836409691228,3.06441356926972));
#9863=CARTESIAN_POINT('Ctrl Pts',(3.47839281480679,-1.17026466187944,3.06335969819392));
#9864=CARTESIAN_POINT('Ctrl Pts',(3.47199232649376,-1.16137818478592,3.06266859060035));
#9865=CARTESIAN_POINT('Ctrl Pts',(3.41001149017844,-1.07381188205242,3.05594155443617));
#9866=CARTESIAN_POINT('Ctrl Pts',(3.3601185833546,-0.991245064867244,3.05024775519266));
#9867=CARTESIAN_POINT('Ctrl Pts',(3.25811809403412,-0.790998727362796,3.03713318581263));
#9868=CARTESIAN_POINT('Ctrl Pts',(3.21103261191144,-0.671260268431884,3.02978328090813));
#9869=CARTESIAN_POINT('Ctrl Pts',(3.15908950397202,-0.489398099386128,3.0184763793657));
#9870=CARTESIAN_POINT('Ctrl Pts',(3.14508067327121,-0.430239871078381,3.01478114614464));
#9871=CARTESIAN_POINT('Ctrl Pts',(3.13098495275062,-0.355677914969023,3.01005782073257));
#9872=CARTESIAN_POINT('Ctrl Pts',(3.12834476129221,-0.34078619450181,3.00911130865941));
#9873=CARTESIAN_POINT('Ctrl Pts',(3.12440111726925,-0.316969960479531,3.00759191887856));
#9874=CARTESIAN_POINT('Ctrl Pts',(3.12298838078027,-0.308063947360792,3.00702249511245));
#9875=CARTESIAN_POINT('Ctrl Pts',(3.1204282420379,-0.291185781348925,3.0059408561587));
#9876=CARTESIAN_POINT('Ctrl Pts',(3.11926864046898,-0.283215639618584,3.00542903666978));
#9877=CARTESIAN_POINT('Ctrl Pts',(3.11674790692168,-0.265121761263558,3.00426461682406));
#9878=CARTESIAN_POINT('Ctrl Pts',(3.11541621566462,-0.254994216013902,3.00361110521924));
#9879=CARTESIAN_POINT('Ctrl Pts',(3.11217314627363,-0.228774058520256,3.00191442383744));
#9880=CARTESIAN_POINT('Ctrl Pts',(3.11038001797486,-0.212667837621573,3.00086758918041));
#9881=CARTESIAN_POINT('Ctrl Pts',(3.09595363973842,-0.0669636060906816,
2.99135374193094));
#9882=CARTESIAN_POINT('Ctrl Pts',(3.09584453860064,0.0635354900294857,2.98248929467057));
#9883=CARTESIAN_POINT('Ctrl Pts',(3.11746786251759,0.285867328631664,2.96697124783214));
#9884=CARTESIAN_POINT('Ctrl Pts',(3.1329827000008,0.377896337761139,2.96043185371752));
#9885=CARTESIAN_POINT('Ctrl Pts',(3.16869435037146,0.525692624310654,2.94998233966712));
#9886=CARTESIAN_POINT('Ctrl Pts',(3.18503757925898,0.582248075434627,2.94599874786823));
#9887=CARTESIAN_POINT('Ctrl Pts',(3.20703853202009,0.647421863521953,2.94148705687845));
#9888=CARTESIAN_POINT('Ctrl Pts',(3.21028839902287,0.656816672823371,2.94083867070505));
#9889=CARTESIAN_POINT('Ctrl Pts',(3.2153949322283,0.67122914100788,2.93984745554976));
#9890=CARTESIAN_POINT('Ctrl Pts',(3.21720172264121,0.676264122610122,2.93950182987135));
#9891=CARTESIAN_POINT('Ctrl Pts',(3.22056535742885,0.68552026901011,2.9388677289042));
#9892=CARTESIAN_POINT('Ctrl Pts',(3.22211622294915,0.689743422617815,2.93857892107796));
#9893=CARTESIAN_POINT('Ctrl Pts',(3.22565493313783,0.699279837056318,2.93792787093746));
#9894=CARTESIAN_POINT('Ctrl Pts',(3.22765116042811,0.704589880881847,2.93756612945849));
#9895=CARTESIAN_POINT('Ctrl Pts',(3.23286804383442,0.718289286317735,2.93663469861728));
#9896=CARTESIAN_POINT('Ctrl Pts',(3.23612282643017,0.726665636302621,2.93606696301326));
#9897=CARTESIAN_POINT('Ctrl Pts',(3.25749507185824,0.780586003006086,2.93242206647504));
#9898=CARTESIAN_POINT('Ctrl Pts',(3.27723098210347,0.825475159389581,2.92943255026893));
#9899=CARTESIAN_POINT('Ctrl Pts',(3.37231660202252,1.02177341304041,2.91636802706252));
#9900=CARTESIAN_POINT('Ctrl Pts',(3.46508258026458,1.16396660454672,2.90687021929907));
#9901=CARTESIAN_POINT('Ctrl Pts',(3.61895713219339,1.34478741498196,2.89274301742363));
#9902=CARTESIAN_POINT('Ctrl Pts',(3.66587144617644,1.39450198536912,2.88860448416378));
#9903=CARTESIAN_POINT('Ctrl Pts',(3.72655178170956,1.45252558506473,2.88338228307836));
#9904=CARTESIAN_POINT('Ctrl Pts',(3.73799037163492,1.463208500751,2.8824032881618));
#9905=CARTESIAN_POINT('Ctrl Pts',(3.75630075950714,1.47991017023988,2.88084396455564));
#9906=CARTESIAN_POINT('Ctrl Pts',(3.76309037759503,1.48601836981163,2.88026741911284));
#9907=CARTESIAN_POINT('Ctrl Pts',(3.77593302540604,1.49741350722789,2.87917984546561));
#9908=CARTESIAN_POINT('Ctrl Pts',(3.78197654455625,1.50271092404523,2.87866926861631));
#9909=CARTESIAN_POINT('Ctrl Pts',(3.79563606257786,1.51453890628871,2.87751788732708));
#9910=CARTESIAN_POINT('Ctrl Pts',(3.80326960575692,1.52104878854996,2.87687625116742));
#9911=CARTESIAN_POINT('Ctrl Pts',(3.82290044704847,1.53753580025171,2.87523058519151));
#9912=CARTESIAN_POINT('Ctrl Pts',(3.83496612071126,1.54743009778423,2.87422324816928));
#9913=CARTESIAN_POINT('Ctrl Pts',(3.91518493465625,1.61165334281457,2.86755155803434));
#9914=CARTESIAN_POINT('Ctrl Pts',(3.98671096669044,1.66159984981628,2.86171672934004));
#9915=CARTESIAN_POINT('Ctrl Pts',(4.18664148247596,1.78255849078888,2.84572345620774));
#9916=CARTESIAN_POINT('Ctrl Pts',(4.31998406317598,1.84435992113757,2.8353491403926));
#9917=CARTESIAN_POINT('Ctrl Pts',(4.50664533268357,1.90703516887904,2.82188325092822));
#9918=CARTESIAN_POINT('Ctrl Pts',(4.55499925611224,1.92125767938949,2.81848891847914));
#9919=CARTESIAN_POINT('Ctrl Pts',(4.61312170891715,1.93598590843416,2.81455903386999));
#9920=CARTESIAN_POINT('Ctrl Pts',(4.62241636720697,1.93827011571675,2.81393510606344));
#9921=CARTESIAN_POINT('Ctrl Pts',(4.63685397554141,1.94170822945358,2.81297332097893));
#9922=CARTESIAN_POINT('Ctrl Pts',(4.64198551497529,1.94290876496222,2.81263291476507));
#9923=CARTESIAN_POINT('Ctrl Pts',(4.65151352693363,1.9450980751337,2.8120036089029));
#9924=CARTESIAN_POINT('Ctrl Pts',(4.6559085648697,1.94609228365405,2.81171441521704));
#9925=CARTESIAN_POINT('Ctrl Pts',(4.66594598226418,1.948327138278,2.81105640385118));
#9926=CARTESIAN_POINT('Ctrl Pts',(4.67159040391613,1.94955817142729,2.81068813409623));
#9927=CARTESIAN_POINT('Ctrl Pts',(4.68636655974522,1.95271362843127,2.80972846134835));
#9928=CARTESIAN_POINT('Ctrl Pts',(4.6955067127439,1.95459854818002,2.80913921416225));
#9929=CARTESIAN_POINT('Ctrl Pts',(4.75989782562752,1.96740710543544,2.80501667984474));
#9930=CARTESIAN_POINT('Ctrl Pts',(4.8155818987722,1.97605170724412,2.80159937169849));
#9931=CARTESIAN_POINT('Ctrl Pts',(5.03278783868504,2.00040550833585,2.78858259232941));
#9932=CARTESIAN_POINT('Ctrl Pts',(5.1956190018227,1.99874752598073,2.77944096667626));
#9933=CARTESIAN_POINT('Ctrl Pts',(5.42319181716855,1.968521876308,2.76577320499344));
#9934=CARTESIAN_POINT('Ctrl Pts',(5.4894274722456,1.95628689666896,2.76169307408302));
#9935=CARTESIAN_POINT('Ctrl Pts',(5.57007738013882,1.93712576051797,2.75653651207407));
#9936=CARTESIAN_POINT('Ctrl Pts',(5.58519827033156,1.93334551863264,2.75556152719567));
#9937=CARTESIAN_POINT('Ctrl Pts',(5.60909283176573,1.92707342748075,2.75400713282003));
#9938=CARTESIAN_POINT('Ctrl Pts',(5.61789658436368,1.92469788312874,2.75343146523104));
#9939=CARTESIAN_POINT('Ctrl Pts',(5.63442995422656,1.9201147864167,2.75234464410352));
#9940=CARTESIAN_POINT('Ctrl Pts',(5.64216314013123,1.91792070322963,2.75183393515021));
#9941=CARTESIAN_POINT('Ctrl Pts',(5.65953790316027,1.91287741073224,2.75068104842828));
#9942=CARTESIAN_POINT('Ctrl Pts',(5.66917157009502,1.91000194685948,2.75003802968309));
#9943=CARTESIAN_POINT('Ctrl Pts',(5.69376724371163,1.90245764920388,2.74838644681994));
#9944=CARTESIAN_POINT('Ctrl Pts',(5.70869648510636,1.89768514268986,2.747374534872));
#9945=CARTESIAN_POINT('Ctrl Pts',(5.80838310915044,1.8645179949319,2.74055292250614));
#9946=CARTESIAN_POINT('Ctrl Pts',(5.89119397304827,1.83063371061706,2.73456351267928));
#9947=CARTESIAN_POINT('Ctrl Pts',(6.08862499505134,1.73390653964181,2.71950039032983));
#9948=CARTESIAN_POINT('Ctrl Pts',(6.19988048016363,1.66514189927543,2.71029725601398));
#9949=CARTESIAN_POINT('Ctrl Pts',(6.35380942151657,1.54772632456468,2.69696348222466));
#9950=CARTESIAN_POINT('Ctrl Pts',(6.40215819008974,1.50707786112066,2.69267921460158));
#9951=CARTESIAN_POINT('Ctrl Pts',(6.45591381809099,1.45734328249231,2.68787443786638));
#9952=CARTESIAN_POINT('Ctrl Pts',(6.46327358152506,1.45042959702501,2.68721568019898));
#9953=CARTESIAN_POINT('Ctrl Pts',(6.47447565518848,1.43974520457679,2.68621201132708));
#9954=CARTESIAN_POINT('Ctrl Pts',(6.4783556027667,1.43601445471509,2.68586419540469));
#9955=CARTESIAN_POINT('Ctrl Pts',(6.48544936121748,1.42913799949735,2.6852280181593));
#9956=CARTESIAN_POINT('Ctrl Pts',(6.48866763111459,1.4259971365444,2.6849393083289));
#9957=CARTESIAN_POINT('Ctrl Pts',(6.49589303829415,1.4188976525757,2.68429089195976));
#9958=CARTESIAN_POINT('Ctrl Pts',(6.49989404108337,1.41493293244304,2.68393166800227));
#9959=CARTESIAN_POINT('Ctrl Pts',(6.51162481018724,1.40320964734802,2.68287773979697));
#9960=CARTESIAN_POINT('Ctrl Pts',(6.5193076839296,1.3954041636229,2.68218658569109));
#9961=CARTESIAN_POINT('Ctrl Pts',(6.58997112855875,1.3224203012347,2.67581665945378));
#9962=CARTESIAN_POINT('Ctrl Pts',(6.64851364673704,1.25307480858604,2.67044020763134));
#9963=CARTESIAN_POINT('Ctrl Pts',(6.77105887491358,1.08604530044307,2.6583279921024));
#9964=CARTESIAN_POINT('Ctrl Pts',(6.83161250615947,0.986256831199962,2.65165598822264));
#9965=CARTESIAN_POINT('Ctrl Pts',(6.9054471220186,0.83642926150532,2.64176352143123));
#9966=CARTESIAN_POINT('Ctrl Pts',(6.92605152991183,0.790274706547201,2.63873414397802));
#9967=CARTESIAN_POINT('Ctrl Pts',(6.95737388764499,0.712281517808107,2.63360407835666));
#9968=CARTESIAN_POINT('Ctrl Pts',(6.96908038201041,0.680864536925153,2.63153491007232));
#9969=CARTESIAN_POINT('Ctrl Pts',(6.98399671548727,0.637525085206788,2.62866991586266));
#9970=CARTESIAN_POINT('Ctrl Pts',(6.98789622605157,0.625844665196475,2.62789675047019));
#9971=CARTESIAN_POINT('Ctrl Pts',(6.99427660058254,0.606127217380235,2.62658954571154));
#9972=CARTESIAN_POINT('Ctrl Pts',(6.99681526420447,0.59810914688202,2.62605740915565));
#9973=CARTESIAN_POINT('Ctrl Pts',(7.00173461335333,0.582223546202908,2.62500190724928));
#9974=CARTESIAN_POINT('Ctrl Pts',(7.00411752627149,0.574356876437284,2.62447862666401));
#9975=CARTESIAN_POINT('Ctrl Pts',(7.00979504117397,0.555187558878182,2.62320197283816));
#9976=CARTESIAN_POINT('Ctrl Pts',(7.0130383001815,0.543870146993055,2.62244695243635));
#9977=CARTESIAN_POINT('Ctrl Pts',(7.02196835379593,0.511633674051969,2.62029237784176));
#9978=CARTESIAN_POINT('Ctrl Pts',(7.0274144415132,0.490650224892829,2.6188851642908));
#9979=CARTESIAN_POINT('Ctrl Pts',(7.06976555882728,0.315802071986491,2.60711631059225));
#9980=CARTESIAN_POINT('Ctrl Pts',(7.08857715545311,0.158164798835133,2.59616345434794));
#9981=CARTESIAN_POINT('Ctrl Pts',(7.08857715545311,-4.46165673850807E-12,
2.58513735103561));
#9982=CARTESIAN_POINT('',(7.08857712267632,0.00123466570667409,2.42852336023369));
#9983=CARTESIAN_POINT('Ctrl Pts',(7.08857715545311,3.31900585956301E-12,
2.42843892255116));
#9984=CARTESIAN_POINT('Ctrl Pts',(7.08857715545311,0.000410617190948955,
2.428467208281));
#9985=CARTESIAN_POINT('Ctrl Pts',(7.08857702866544,0.000821238121669504,
2.42849549165351));
#9986=CARTESIAN_POINT('Ctrl Pts',(7.08857677508315,0.00123186273744409,
2.4285237726487));
#9987=CARTESIAN_POINT('Ctrl Pts',(7.08857677337603,0.00123462397966759,
2.428523962824));
#9988=CARTESIAN_POINT('Ctrl Pts',(7.08854025465424,0.0602369660175714,2.43258763604517));
#9989=CARTESIAN_POINT('Ctrl Pts',(7.08588590411455,0.11921567211675,2.43659616672538));
#9990=CARTESIAN_POINT('Ctrl Pts',(7.07982904186567,0.186822369557015,2.44106952969729));
#9991=CARTESIAN_POINT('Ctrl Pts',(7.07897947661117,0.195643448811554,2.44165079025752));
#9992=CARTESIAN_POINT('Ctrl Pts',(7.0774927640007,0.210071789148959,2.44259727988455));
#9993=CARTESIAN_POINT('Ctrl Pts',(7.07689056797417,0.215682421341409,2.44296427802026));
#9994=CARTESIAN_POINT('Ctrl Pts',(7.07577889611734,0.225641366031836,2.44361373954427));
#9995=CARTESIAN_POINT('Ctrl Pts',(7.07527890133582,0.229990669398404,2.44389670823432));
#9996=CARTESIAN_POINT('Ctrl Pts',(7.07423565016347,0.23880960736887,2.44446907431109));
#9997=CARTESIAN_POINT('Ctrl Pts',(7.0736915773188,0.243279071926444,2.44475841505161));
#9998=CARTESIAN_POINT('Ctrl Pts',(7.07247342880585,0.253011135887692,2.44538682755914));
#9999=CARTESIAN_POINT('Ctrl Pts',(7.07179349041179,0.258272896908093,2.44572556924882));
#10000=CARTESIAN_POINT('Ctrl Pts',(7.06984161628269,0.272917698420617,2.44666569445789));
#10001=CARTESIAN_POINT('Ctrl Pts',(7.06852383276362,0.282294634217964,2.44726458370449));
#10002=CARTESIAN_POINT('Ctrl Pts',(7.06090677652683,0.333829722981961,2.45054092490055));
#10003=CARTESIAN_POINT('Ctrl Pts',(7.0533237140759,0.375790299831245,2.4531528836701));
#10004=CARTESIAN_POINT('Ctrl Pts',(7.03617895593015,0.455895236060439,2.45808706384697));
#10005=CARTESIAN_POINT('Ctrl Pts',(7.02682325599828,0.494062076019784,2.46041483374894));
#10006=CARTESIAN_POINT('Ctrl Pts',(6.97717417179435,0.673505670480455,2.47135044457464));
#10007=CARTESIAN_POINT('Ctrl Pts',(6.92248551594705,0.810317777363745,2.47969874679399));
#10008=CARTESIAN_POINT('Ctrl Pts',(6.82528461060875,0.992275397383697,2.49204252896068));
#10009=CARTESIAN_POINT('Ctrl Pts',(6.79497509402291,1.04338394583525,2.49565684294258));
#10010=CARTESIAN_POINT('Ctrl Pts',(6.75420306693964,1.10562423997621,2.50028890785388));
#10011=CARTESIAN_POINT('Ctrl Pts',(6.74583177967914,1.11809383757276,2.50122895193193));
#10012=CARTESIAN_POINT('Ctrl Pts',(6.73222337040408,1.13787798274131,2.50274038960131));
#10013=CARTESIAN_POINT('Ctrl Pts',(6.72707608773023,1.14525385033864,2.50330839331741));
#10014=CARTESIAN_POINT('Ctrl Pts',(6.71722294491025,1.15917151883042,2.50438889899884));
#10015=CARTESIAN_POINT('Ctrl Pts',(6.7125269701184,1.16572012343655,2.50490101658599));
#10016=CARTESIAN_POINT('Ctrl Pts',(6.7017655676926,1.18053664528241,2.50606827962637));
#10017=CARTESIAN_POINT('Ctrl Pts',(6.69567584613039,1.18878655532312,2.50672435350424));
#10018=CARTESIAN_POINT('Ctrl Pts',(6.67971996387891,1.21005720412223,2.50843210131766));
#10019=CARTESIAN_POINT('Ctrl Pts',(6.66975713222072,1.22300413701099,2.50948751994744));
#10020=CARTESIAN_POINT('Ctrl Pts',(6.58453981323938,1.33097563636166,2.51842675531303));
#10021=CARTESIAN_POINT('Ctrl Pts',(6.50094015791897,1.41906449691718,2.52665148109656));
#10022=CARTESIAN_POINT('Ctrl Pts',(6.30055901765953,1.59498853664329,2.54513649478515));
#10023=CARTESIAN_POINT('Ctrl Pts',(6.18106484259249,1.67872213949061,2.55542696833088));
#10024=CARTESIAN_POINT('Ctrl Pts',(6.04127764800335,1.75543733407049,2.56605223437323));
#10025=CARTESIAN_POINT('Ctrl Pts',(6.02896176303418,1.76202893267157,2.5669768994246));
#10026=CARTESIAN_POINT('Ctrl Pts',(6.0070920256358,1.77343996331735,2.56859741021253));
#10027=CARTESIAN_POINT('Ctrl Pts',(5.99756685486375,1.77831285054461,2.5692961234726));
#10028=CARTESIAN_POINT('Ctrl Pts',(5.98309796682004,1.78556856277171,2.57034628803498));
#10029=CARTESIAN_POINT('Ctrl Pts',(5.97818304460048,1.78800792262705,2.57070107958827));
#10030=CARTESIAN_POINT('Ctrl Pts',(5.97324458884348,1.79043361803056,2.57105558400338));
#10031=CARTESIAN_POINT('Ctrl Pts',(5.97323112840455,1.79044022940787,2.57105655023906));
#10032=CARTESIAN_POINT('Ctrl Pts',(5.97320487235439,1.7904531252509,2.57105843495803));
#10033=CARTESIAN_POINT('Ctrl Pts',(5.97319207673019,1.79045940974114,2.57105935344368));
#10034=CARTESIAN_POINT('Ctrl Pts',(5.97316632002369,1.7904720596426,2.57106120226492));
#10035=CARTESIAN_POINT('Ctrl Pts',(5.97315335899579,1.79047842502269,2.57106213259625));
#10036=CARTESIAN_POINT('Ctrl Pts',(5.9731272691552,1.79049123783319,2.57106400527479));
#10037=CARTESIAN_POINT('Ctrl Pts',(5.9731141402062,1.790497685326,2.57106494763144));
#10038=CARTESIAN_POINT('Ctrl Pts',(5.97308771195149,1.79051066361127,2.57106684454415));
#10039=CARTESIAN_POINT('Ctrl Pts',(5.97307441275842,1.79051719434375,2.57106779909176));
#10040=CARTESIAN_POINT('Ctrl Pts',(5.9730476414839,1.79053034033748,2.571069720567));
#10041=CARTESIAN_POINT('Ctrl Pts',(5.97303416942019,1.79053695558521,2.57107068749298));
#10042=CARTESIAN_POINT('Ctrl Pts',(5.97300704989647,1.79055027182643,2.57107263390383));
#10043=CARTESIAN_POINT('Ctrl Pts',(5.97299340243132,1.79055697281751,2.57107361338868));
#10044=CARTESIAN_POINT('Ctrl Pts',(5.97296592951168,1.79057046180373,2.57107558510219));
#10045=CARTESIAN_POINT('Ctrl Pts',(5.9729521040551,1.79057724979481,2.57107657733061));
#10046=CARTESIAN_POINT('Ctrl Pts',(5.97292427250901,1.79059091406369,2.57107857471978));
#10047=CARTESIAN_POINT('Ctrl Pts',(5.97291026641626,1.79059779033785,2.57107957988036));
#10048=CARTESIAN_POINT('Ctrl Pts',(5.97288207093768,1.79061163246313,2.57108160332353));
#10049=CARTESIAN_POINT('Ctrl Pts',(5.97286788150617,1.79061859833131,2.57108262160898));
#10050=CARTESIAN_POINT('Ctrl Pts',(5.97283931657448,1.79063262099103,2.57108467149981));
#10051=CARTESIAN_POINT('Ctrl Pts',(5.97282494111046,1.7906396777593,2.57108570310216));
#10052=CARTESIAN_POINT('Ctrl Pts',(5.97279600138937,1.79065388353995,2.57108777982099));
#10053=CARTESIAN_POINT('Ctrl Pts',(5.97278143704024,1.79066103259184,2.57108882494363));
#10054=CARTESIAN_POINT('Ctrl Pts',(5.97275211664794,1.7906754243466,2.57109092890986));
#10055=CARTESIAN_POINT('Ctrl Pts',(5.97273736068233,1.79068266700555,2.57109198774744));
#10056=CARTESIAN_POINT('Ctrl Pts',(5.9727076541774,1.79069724737028,2.57109411934879));
#10057=CARTESIAN_POINT('Ctrl Pts',(5.97269270363054,1.79070458507375,2.57109519211264));
#10058=CARTESIAN_POINT('Ctrl Pts',(5.9726626050891,1.79071935691996,2.57109735177134));
#10059=CARTESIAN_POINT('Ctrl Pts',(5.97264745704566,1.79072679108051,2.57109843866922));
#10060=CARTESIAN_POINT('Ctrl Pts',(5.97261696048989,1.79074175730498,2.57110062681131));
#10061=CARTESIAN_POINT('Ctrl Pts',(5.97260161200983,1.79074928934671,2.57110172805269));
#10062=CARTESIAN_POINT('Ctrl Pts',(5.97257071151941,1.79076445281675,2.57110394509994));
#10063=CARTESIAN_POINT('Ctrl Pts',(5.9725551595434,1.79077208422166,2.57110506090282));
#10064=CARTESIAN_POINT('Ctrl Pts',(5.97252384899427,1.79078744790328,2.57110730729155));
#10065=CARTESIAN_POINT('Ctrl Pts',(5.97250809042578,1.790795180171,2.57110843787653));
#10066=CARTESIAN_POINT('Ctrl Pts',(5.97247636356511,1.79081074709209,2.57111071405217));
#10067=CARTESIAN_POINT('Ctrl Pts',(5.97246039527237,1.79081858173883,2.57111185964233));
#10068=CARTESIAN_POINT('Ctrl Pts',(5.97242824583908,1.79083435492997,2.57111416605082));
#10069=CARTESIAN_POINT('Ctrl Pts',(5.9724120645942,1.79084229351844,2.57111532687608));
#10070=CARTESIAN_POINT('Ctrl Pts',(5.97237948594145,1.79085827619806,2.57111766399092));
#10071=CARTESIAN_POINT('Ctrl Pts',(5.97236308857734,1.79086632026042,2.57111884027678));
#10072=CARTESIAN_POINT('Ctrl Pts',(5.97233007431993,1.79088251551715,2.57112120855257));
#10073=CARTESIAN_POINT('Ctrl Pts',(5.97231345748322,1.79089066667623,2.57112240053785));
#10074=CARTESIAN_POINT('Ctrl Pts',(5.97228000099322,1.79090707771628,2.57112480044649));
#10075=CARTESIAN_POINT('Ctrl Pts',(5.97226316127134,1.79091533762317,2.57112600837418));
#10076=CARTESIAN_POINT('Ctrl Pts',(5.96821033339912,1.79290318438824,2.57141671562544));
#10077=CARTESIAN_POINT('Ctrl Pts',(5.96416771133279,1.79486910055042,2.57170535442568));
#10078=CARTESIAN_POINT('Ctrl Pts',(5.9550843520656,1.79924840843737,2.57235092071349));
#10079=CARTESIAN_POINT('Ctrl Pts',(5.95004010708574,1.80165428905277,2.57270738570606));
#10080=CARTESIAN_POINT('Ctrl Pts',(5.93526624459514,1.80862470384438,2.57374567213332));
#10081=CARTESIAN_POINT('Ctrl Pts',(5.92550959022008,1.81313193117825,2.57442409910285));
#10082=CARTESIAN_POINT('Ctrl Pts',(5.85112314628559,1.8467690249183,2.57954517206707));
#10083=CARTESIAN_POINT('Ctrl Pts',(5.78501070564641,1.87251719591821,2.58380417035013));
#10084=CARTESIAN_POINT('Ctrl Pts',(5.57591679250681,1.94136201753426,2.59679114563572));
#10085=CARTESIAN_POINT('Ctrl Pts',(5.42938558965196,1.97197852233778,2.60525083148297));
#10086=CARTESIAN_POINT('Ctrl Pts',(5.21596457167497,1.99207225382881,2.61803044648524));
#10087=CARTESIAN_POINT('Ctrl Pts',(5.15086762364297,1.99499736680657,2.62198219059259));
#10088=CARTESIAN_POINT('Ctrl Pts',(5.0703103922254,1.99467111801823,2.62699437735823));
#10089=CARTESIAN_POINT('Ctrl Pts',(5.05487370116904,1.99442937066823,2.62796026857337));
#10090=CARTESIAN_POINT('Ctrl Pts',(5.03035874410439,1.99376073910522,2.62950348399473));
#10091=CARTESIAN_POINT('Ctrl Pts',(5.02127770633231,1.99345095175818,2.63007715932044));
#10092=CARTESIAN_POINT('Ctrl Pts',(5.00416303744325,1.99275000866163,2.63116229374953));
#10093=CARTESIAN_POINT('Ctrl Pts',(4.99612901532178,1.99237228484056,2.63167332372166));
#10094=CARTESIAN_POINT('Ctrl Pts',(4.97800871792434,1.99141048610662,2.63282972919786));
#10095=CARTESIAN_POINT('Ctrl Pts',(4.96792421401502,1.99079835186766,2.6334759672314));
#10096=CARTESIAN_POINT('Ctrl Pts',(4.9420457067158,1.98903009924406,2.63514134963781));
#10097=CARTESIAN_POINT('Ctrl Pts',(4.92626027352336,1.98776247576293,2.63616393745795));
#10098=CARTESIAN_POINT('Ctrl Pts',(4.81660022527514,1.97764090637914,2.64331612899059));
#10099=CARTESIAN_POINT('Ctrl Pts',(4.72345497253705,1.96232978470293,2.64964664342784));
#10100=CARTESIAN_POINT('Ctrl Pts',(4.46558455054291,1.90092509648242,2.6678489034237));
#10101=CARTESIAN_POINT('Ctrl Pts',(4.30519573921176,1.84018037944455,2.68002429642541));
#10102=CARTESIAN_POINT('Ctrl Pts',(4.14103046651171,1.75255227848553,2.69245390366278));
#10103=CARTESIAN_POINT('Ctrl Pts',(4.12763389415773,1.74520246166273,2.69346737338104));
#10104=CARTESIAN_POINT('Ctrl Pts',(4.10422803508306,1.7320090711367,2.69523487934507));
#10105=CARTESIAN_POINT('Ctrl Pts',(4.09418289347302,1.72623092496356,2.69599239588305));
#10106=CARTESIAN_POINT('Ctrl Pts',(4.07928268657311,1.71748637199194,2.69711382419378));
#10107=CARTESIAN_POINT('Ctrl Pts',(4.0743892422171,1.71458632337467,2.69748175768301));
#10108=CARTESIAN_POINT('Ctrl Pts',(4.06601692985436,1.70957604591039,2.6981105561612));
#10109=CARTESIAN_POINT('Ctrl Pts',(4.06253204880839,1.70747606737805,2.69837207117033));
#10110=CARTESIAN_POINT('Ctrl Pts',(4.05463896535233,1.70268673908978,2.69896388618684));
#10111=CARTESIAN_POINT('Ctrl Pts',(4.05023476844239,1.6999909285477,2.69929376067777));
#10112=CARTESIAN_POINT('Ctrl Pts',(4.03831176358491,1.69262905642084,2.70018598949965));
#10113=CARTESIAN_POINT('Ctrl Pts',(4.03081335032637,1.68792995177575,2.7007462420798));
#10114=CARTESIAN_POINT('Ctrl Pts',(3.99430943582904,1.6647139447737,2.70347066497373));
#10115=CARTESIAN_POINT('Ctrl Pts',(3.96575326395656,1.64549729812261,2.70559259282032));
#10116=CARTESIAN_POINT('Ctrl Pts',(3.83372494170271,1.55159638194335,2.71543025918857));
#10117=CARTESIAN_POINT('Ctrl Pts',(3.73706923804305,1.46782937716243,2.72272767451616));
#10118=CARTESIAN_POINT('Ctrl Pts',(3.59226287767608,1.31572057686954,2.73495150690417));
#10119=CARTESIAN_POINT('Ctrl Pts',(3.53920861368146,1.25258753812167,2.73978622293921));
#10120=CARTESIAN_POINT('Ctrl Pts',(3.46224533861029,1.14855545618745,2.74759775881338));
#10121=CARTESIAN_POINT('Ctrl Pts',(3.43562538092258,1.10977709690693,2.75047789829529));
#10122=CARTESIAN_POINT('Ctrl Pts',(3.40293399785123,1.05834856148039,2.75427756756005));
#10123=CARTESIAN_POINT('Ctrl Pts',(3.395589492297,1.04652289604748,2.7551499121363));
#10124=CARTESIAN_POINT('Ctrl Pts',(3.38382936967621,1.02713765233417,2.75657817233989));
#10125=CARTESIAN_POINT('Ctrl Pts',(3.37933860295248,1.01962404032246,2.75713133916255));
#10126=CARTESIAN_POINT('Ctrl Pts',(3.37077639267072,1.00508188985476,2.75820127738248));
#10127=CARTESIAN_POINT('Ctrl Pts',(3.36669813326708,0.998057550430446,2.75871778881004));
#10128=CARTESIAN_POINT('Ctrl Pts',(3.35741724544162,0.981845036036596,2.75990932659627));
#10129=CARTESIAN_POINT('Ctrl Pts',(3.35224447945945,0.972640131799848,2.76058540502048));
#10130=CARTESIAN_POINT('Ctrl Pts',(3.33632015842499,0.943768554619699,2.76270485679206));
#10131=CARTESIAN_POINT('Ctrl Pts',(3.32582713832255,0.923962012769674,2.76415729338854));
#10132=CARTESIAN_POINT('Ctrl Pts',(3.23774751296958,0.750707328722994,2.77685355142233));
#10133=CARTESIAN_POINT('Ctrl Pts',(3.17998421767927,0.588026098904509,2.78881017708032));
#10134=CARTESIAN_POINT('Ctrl Pts',(3.1227904194247,0.322480041929148,2.80772939197737));
#10135=CARTESIAN_POINT('Ctrl Pts',(3.10912876871158,0.223508524924275,2.81463375820815));
#10136=CARTESIAN_POINT('Ctrl Pts',(3.10219040185798,0.112037327689403,2.82198497726712));
#10137=CARTESIAN_POINT('Ctrl Pts',(3.10155713214352,0.100147350484549,2.82276361774902));
#10138=CARTESIAN_POINT('Ctrl Pts',(3.10077591496193,0.0825068914882814,
2.82391003553255));
#10139=CARTESIAN_POINT('Ctrl Pts',(3.10054632860217,0.0767605476189505,
2.82428209422477));
#10140=CARTESIAN_POINT('Ctrl Pts',(3.10018124912889,0.0665120219008368,
2.82494309155892));
#10141=CARTESIAN_POINT('Ctrl Pts',(3.10003615021763,0.0620103027300323,
2.82523255062056));
#10142=CARTESIAN_POINT('Ctrl Pts',(3.09975381515558,0.052221162266119,2.82586004781252));
#10143=CARTESIAN_POINT('Ctrl Pts',(3.09962235961899,0.0469336777105539,
2.82619776379596));
#10144=CARTESIAN_POINT('Ctrl Pts',(3.09931575784451,0.0322512211414929,
2.82713231472387));
#10145=CARTESIAN_POINT('Ctrl Pts',(3.09918595962792,0.0228552961052907,
2.82772670261983));
#10146=CARTESIAN_POINT('Ctrl Pts',(3.0988423185119,-0.0280759391005415,
2.83093041953442));
#10147=CARTESIAN_POINT('Ctrl Pts',(3.09985939905145,-0.0696124771190814,
2.83347763134926));
#10148=CARTESIAN_POINT('Ctrl Pts',(3.10371476138736,-0.138732467783235,
2.83765157044059));
#10149=CARTESIAN_POINT('Ctrl Pts',(3.1058319548193,-0.166340697732581,2.83930143894376));
#10150=CARTESIAN_POINT('Ctrl Pts',(3.12099001510693,-0.321543636251902,
2.84852167327295));
#10151=CARTESIAN_POINT('Ctrl Pts',(3.14573828711977,-0.447692461286682,
2.85582655281387));
#10152=CARTESIAN_POINT('Ctrl Pts',(3.19907176998566,-0.626350773667581,
2.86680624526192));
#10153=CARTESIAN_POINT('Ctrl Pts',(3.21814648867054,-0.681347586354424,
2.87027496428726));
#10154=CARTESIAN_POINT('Ctrl Pts',(3.24875820866924,-0.758528614746119,
2.87532707307689));
#10155=CARTESIAN_POINT('Ctrl Pts',(3.25835044303736,-0.781453924566613,
2.87685148876626));
#10156=CARTESIAN_POINT('Ctrl Pts',(3.27621718781569,-0.822010104859998,
2.87959499248833));
#10157=CARTESIAN_POINT('Ctrl Pts',(3.28432643245261,-0.839710485126383,
2.88080857533339));
#10158=CARTESIAN_POINT('Ctrl Pts',(3.29696500487535,-0.866263683693215,
2.88265507955644));
#10159=CARTESIAN_POINT('Ctrl Pts',(3.30130372376113,-0.875206317940565,
2.88328145470455));
#10160=CARTESIAN_POINT('Ctrl Pts',(3.30926779326416,-0.891313589617056,
2.88441801729611));
#10161=CARTESIAN_POINT('Ctrl Pts',(3.31286993493676,-0.898489514592974,
2.8849273905006));
#10162=CARTESIAN_POINT('Ctrl Pts',(3.32069119114078,-0.91383861502776,2.88602353094389));
#10163=CARTESIAN_POINT('Ctrl Pts',(3.32492369564684,-0.922004722049179,
2.88661075804306));
#10164=CARTESIAN_POINT('Ctrl Pts',(3.33645959683618,-0.943890024705633,
2.88819563276008));
#10165=CARTESIAN_POINT('Ctrl Pts',(3.34386698759133,-0.957553394392518,
2.88919692392528));
#10166=CARTESIAN_POINT('Ctrl Pts',(3.38085762267307,-1.0239218124382,2.89411983999269));
#10167=CARTESIAN_POINT('Ctrl Pts',(3.41266341670061,-1.075345389917,2.89812008837174));
#10168=CARTESIAN_POINT('Ctrl Pts',(3.4618976697215,-1.14741214976728,2.90400392478264));
#10169=CARTESIAN_POINT('Ctrl Pts',(3.47748940346697,-1.16927356372593,2.90582767304293));
#10170=CARTESIAN_POINT('Ctrl Pts',(3.58241177300322,-1.31027666671523,2.91784219186277));
#10171=CARTESIAN_POINT('Ctrl Pts',(3.68439504589187,-1.41940055981079,2.92838763838404));
#10172=CARTESIAN_POINT('Ctrl Pts',(3.83609472731421,-1.54909857175908,2.9420397000156));
#10173=CARTESIAN_POINT('Ctrl Pts',(3.87586989730947,-1.58056266122812,2.94545574865899));
#10174=CARTESIAN_POINT('Ctrl Pts',(3.9245437356649,-1.6161360528959,2.94940726466923));
#10175=CARTESIAN_POINT('Ctrl Pts',(3.9323240830601,-1.62173674771662,2.9500322047835));
#10176=CARTESIAN_POINT('Ctrl Pts',(3.94444655995106,-1.63033113721861,2.95099520964631));
#10177=CARTESIAN_POINT('Ctrl Pts',(3.94876056917908,-1.6333639780689,2.95133583339078));
#10178=CARTESIAN_POINT('Ctrl Pts',(3.95678289645264,-1.63895644163596,2.9519653344907));
#10179=CARTESIAN_POINT('Ctrl Pts',(3.96048783734651,-1.64152059236494,2.95225450750159));
#10180=CARTESIAN_POINT('Ctrl Pts',(3.9689591545174,-1.64734114969213,2.9529122080171));
#10181=CARTESIAN_POINT('Ctrl Pts',(3.97373099550769,-1.65058943334688,2.95328018966935));
#10182=CARTESIAN_POINT('Ctrl Pts',(3.98624136165873,-1.65902624292279,2.95423861064149));
#10183=CARTESIAN_POINT('Ctrl Pts',(3.99400235845032,-1.66418141712181,2.9548269033059));
#10184=CARTESIAN_POINT('Ctrl Pts',(4.04861408001894,-1.69990786274216,2.9589248947721));
#10185=CARTESIAN_POINT('Ctrl Pts',(4.09670117803248,-1.72855376961531,2.96232017793692));
#10186=CARTESIAN_POINT('Ctrl Pts',(4.28898747099218,-1.83240114836662,2.97533877869482));
#10187=CARTESIAN_POINT('Ctrl Pts',(4.44095221852488,-1.89188281096374,2.98449851604059));
#10188=CARTESIAN_POINT('Ctrl Pts',(4.66372036696744,-1.94899326999315,2.99818971026618));
#10189=CARTESIAN_POINT('Ctrl Pts',(4.72978198092951,-1.96240574263226,3.0022729535877));
#10190=CARTESIAN_POINT('Ctrl Pts',(4.81180612790805,-1.97477460431549,3.00743301431891));
#10191=CARTESIAN_POINT('Ctrl Pts',(4.82724780242245,-1.97691831513816,3.00840821498446));
#10192=CARTESIAN_POINT('Ctrl Pts',(4.85175953858244,-1.98002878639194,3.00996287468294));
#10193=CARTESIAN_POINT('Ctrl Pts',(4.86081403844431,-1.98111473896125,3.01053858958855));
#10194=CARTESIAN_POINT('Ctrl Pts',(4.87786306924405,-1.9830410209908,3.01162545124521));
#10195=CARTESIAN_POINT('Ctrl Pts',(4.88585587654973,-1.98389518914881,3.0121361530462));
#10196=CARTESIAN_POINT('Ctrl Pts',(4.90385540343027,-1.9857087774684,3.01328895833554));
#10197=CARTESIAN_POINT('Ctrl Pts',(4.91386459368685,-1.98664090508373,3.01393190229928));
#10198=CARTESIAN_POINT('Ctrl Pts',(4.93949285661997,-1.98883232634621,3.01558316478169));
#10199=CARTESIAN_POINT('Ctrl Pts',(4.95512026702194,-1.98998328486813,3.01659482892399));
#10200=CARTESIAN_POINT('Ctrl Pts',(5.05986649364596,-1.99645803224626,3.02340905093284));
#10201=CARTESIAN_POINT('Ctrl Pts',(5.14923040694753,-1.9959770926576,3.02939085914628));
#10202=CARTESIAN_POINT('Ctrl Pts',(5.36849496993185,-1.98006007821124,3.04445245449078));
#10203=CARTESIAN_POINT('Ctrl Pts',(5.49748546654194,-1.95783991751101,3.05366260617979));
#10204=CARTESIAN_POINT('Ctrl Pts',(5.68424947629233,-1.90641437568253,3.06700446626609));
#10205=CARTESIAN_POINT('Ctrl Pts',(5.74430106366956,-1.88676963982752,3.07128995911322));
#10206=CARTESIAN_POINT('Ctrl Pts',(5.81276277897269,-1.86071521220755,3.07609592541344));
#10207=CARTESIAN_POINT('Ctrl Pts',(5.82217324975735,-1.85705183257374,3.07675472287846));
#10208=CARTESIAN_POINT('Ctrl Pts',(5.83655672417828,-1.85132636859108,3.07775843954569));
#10209=CARTESIAN_POINT('Ctrl Pts',(5.84154971322237,-1.84931541753976,3.07810626388341));
#10210=CARTESIAN_POINT('Ctrl Pts',(5.85069908350851,-1.84558735085988,3.07874244922983));
#10211=CARTESIAN_POINT('Ctrl Pts',(5.85485779200564,-1.84387639394661,3.07903115880679));
#10212=CARTESIAN_POINT('Ctrl Pts',(5.86421235132211,-1.83999074362486,3.0796795655577));
#10213=CARTESIAN_POINT('Ctrl Pts',(5.86940479118589,-1.83780810191284,3.08003878021826));
#10214=CARTESIAN_POINT('Ctrl Pts',(5.88466537792273,-1.83131712022219,3.08109265535501));
#10215=CARTESIAN_POINT('Ctrl Pts',(5.89470756246268,-1.82694774838943,3.08178376622395));
#10216=CARTESIAN_POINT('Ctrl Pts',(5.99276773422059,-1.78331765777382,3.08851369443884));
#10217=CARTESIAN_POINT('Ctrl Pts',(6.07787944457729,-1.73780383528504,3.09421005098518));
#10218=CARTESIAN_POINT('Ctrl Pts',(6.26786664299274,-1.61775420838623,3.10732500136062));
#10219=CARTESIAN_POINT('Ctrl Pts',(6.36948383709108,-1.53889451260489,3.11467295179483));
#10220=CARTESIAN_POINT('Ctrl Pts',(6.50701255032076,-1.4091225206863,3.12597722672863));
#10221=CARTESIAN_POINT('Ctrl Pts',(6.54927190348036,-1.36542987486289,3.12967195506992));
#10222=CARTESIAN_POINT('Ctrl Pts',(6.59947559741968,-1.30854080624874,3.13439471140967));
#10223=CARTESIAN_POINT('Ctrl Pts',(6.60935274254128,-1.29708845014935,3.1353411837816));
#10224=CARTESIAN_POINT('Ctrl Pts',(6.62490970612298,-1.27863016397478,3.1368605248164));
#10225=CARTESIAN_POINT('Ctrl Pts',(6.63067400923459,-1.27169596087608,3.13742993993294));
#10226=CARTESIAN_POINT('Ctrl Pts',(6.64149753611098,-1.25849466585887,3.13851157204442));
#10227=CARTESIAN_POINT('Ctrl Pts',(6.64656621782396,-1.25223553385189,3.13902339341002));
#10228=CARTESIAN_POINT('Ctrl Pts',(6.65797719607487,-1.2379687227946,3.14018783073169));
#10229=CARTESIAN_POINT('Ctrl Pts',(6.66429612700988,-1.22994272678768,3.14084135804056));
#10230=CARTESIAN_POINT('Ctrl Pts',(6.6804801035732,-1.20905857178749,3.14253810697932));
#10231=CARTESIAN_POINT('Ctrl Pts',(6.69025043562454,-1.19612829274047,3.14358499397311));
#10232=CARTESIAN_POINT('Ctrl Pts',(6.77707964881563,-1.07825743907066,3.15309774340971));
#10233=CARTESIAN_POINT('Ctrl Pts',(6.84383539292177,-0.966145859060132,
3.16196092255532));
#10234=CARTESIAN_POINT('Ctrl Pts',(6.93881071945174,-0.764030992167013,
3.17747451671486));
#10235=CARTESIAN_POINT('Ctrl Pts',(6.97247817385822,-0.677036552294206,
3.18401069335264));
#10236=CARTESIAN_POINT('Ctrl Pts',(7.01730257704336,-0.531731298182875,
3.1944613813244));
#10237=CARTESIAN_POINT('Ctrl Pts',(7.03216384096697,-0.474708524401591,
3.19844902578721));
#10238=CARTESIAN_POINT('Ctrl Pts',(7.04655994670518,-0.407383197353299,
3.20296468330791));
#10239=CARTESIAN_POINT('Ctrl Pts',(7.04856635010261,-0.397644457040907,
3.20361321800442));
#10240=CARTESIAN_POINT('Ctrl Pts',(7.05154018537318,-0.382643273280248,
3.20460461165063));
#10241=CARTESIAN_POINT('Ctrl Pts',(7.05255937194231,-0.377391425196362,
3.204950268831));
#10242=CARTESIAN_POINT('Ctrl Pts',(7.0543967409988,-0.367715519263763,3.20558439946568));
#10243=CARTESIAN_POINT('Ctrl Pts',(7.05522108325874,-0.363292806948913,
3.20587320568759));
#10244=CARTESIAN_POINT('Ctrl Pts',(7.05705093917638,-0.353287575604664,
3.20652421702005));
#10245=CARTESIAN_POINT('Ctrl Pts',(7.05804760793636,-0.347703540396118,
3.20688592156302));
#10246=CARTESIAN_POINT('Ctrl Pts',(7.06056132531484,-0.333264135557118,
3.2078171931973));
#10247=CARTESIAN_POINT('Ctrl Pts',(7.06204241067935,-0.324402520241099,
3.20838480764394));
#10248=CARTESIAN_POINT('Ctrl Pts',(7.07121065860102,-0.267171646286709,
3.2120271465433));
#10249=CARTESIAN_POINT('Ctrl Pts',(7.07717478455331,-0.218538906957556,
3.21501436720786));
#10250=CARTESIAN_POINT('Ctrl Pts',(7.08249696326586,-0.156217553636739,
3.21876095816004));
#10251=CARTESIAN_POINT('Ctrl Pts',(7.08351321701481,-0.142691686145127,
3.21956921403908));
#10252=CARTESIAN_POINT('Ctrl Pts',(7.08714366116788,-0.0867390665351364,
3.22289626608107));
#10253=CARTESIAN_POINT('Ctrl Pts',(7.08853944685439,-0.0442432801139429,
3.22538421847911));
#10254=CARTESIAN_POINT('Ctrl Pts',(7.08857690420624,-0.00115606523612509,
3.22789393898319));
#10255=CARTESIAN_POINT('Ctrl Pts',(7.08857715545314,-0.000578028495419831,
3.22792760577034));
#10256=CARTESIAN_POINT('Ctrl Pts',(7.08857715545311,9.38914434820126E-11,
3.22796126976449));
#10257=CARTESIAN_POINT('Origin',(5.09382715545311,0.,-6.77268258743872));
#10258=CARTESIAN_POINT('',(7.08857715545311,-9.37345802482419E-11,4.18476380915572));
#10259=CARTESIAN_POINT('',(7.08857715495348,4.36882467403433E-5,4.02544645345466));
#10260=CARTESIAN_POINT('',(7.08857715545311,8.3550772080578E-14,-6.77268258743872));
#10261=CARTESIAN_POINT('Ctrl Pts',(7.08857715545311,-9.37346381069126E-11,
4.18476380915572));
#10262=CARTESIAN_POINT('Ctrl Pts',(7.08857715544518,-0.168685457521296,
4.17493968220012));
#10263=CARTESIAN_POINT('Ctrl Pts',(7.06718218732477,-0.336672456479282,
4.16528040244134));
#10264=CARTESIAN_POINT('Ctrl Pts',(7.01913649669845,-0.522246467177999,
4.15346024509175));
#10265=CARTESIAN_POINT('Ctrl Pts',(7.01298196055782,-0.544428322291977,
4.15202940146003));
#10266=CARTESIAN_POINT('Ctrl Pts',(7.00345982020135,-0.576577096447058,
4.14992716976473));
#10267=CARTESIAN_POINT('Ctrl Pts',(7.00039492180035,-0.586632259583106,
4.14926556326834));
#10268=CARTESIAN_POINT('Ctrl Pts',(6.99482333892916,-0.604406262242485,
4.14808859976392));
#10269=CARTESIAN_POINT('Ctrl Pts',(6.99234873746499,-0.612134967879349,
4.14757429812032));
#10270=CARTESIAN_POINT('Ctrl Pts',(6.9871005811178,-0.628188096590249,4.14650069997607));
#10271=CARTESIAN_POINT('Ctrl Pts',(6.98431912905566,-0.636509734986001,
4.14594115391338));
#10272=CARTESIAN_POINT('Ctrl Pts',(6.97695221431537,-0.658075997784857,
4.14448306267339));
#10273=CARTESIAN_POINT('Ctrl Pts',(6.9722819618218,-0.671290942913361,4.14358174434966));
#10274=CARTESIAN_POINT('Ctrl Pts',(6.95101157132762,-0.729517064067628,
4.13957482989187));
#10275=CARTESIAN_POINT('Ctrl Pts',(6.93293123839276,-0.77396681090106,4.13642065378434));
#10276=CARTESIAN_POINT('Ctrl Pts',(6.8784200460391,-0.895255297385321,4.12754012092097));
#10277=CARTESIAN_POINT('Ctrl Pts',(6.83865537915418,-0.970476976769931,
4.1217134399807));
#10278=CARTESIAN_POINT('Ctrl Pts',(6.72375825304741,-1.15780573846782,4.10646249844511));
#10279=CARTESIAN_POINT('Ctrl Pts',(6.64183531549823,-1.26525226317017,4.09695183356967));
#10280=CARTESIAN_POINT('Ctrl Pts',(6.53240339601693,-1.38208762899703,4.08622313576878));
#10281=CARTESIAN_POINT('Ctrl Pts',(6.51475521064603,-1.40022548848324,4.08454598131497));
#10282=CARTESIAN_POINT('Ctrl Pts',(6.49107387052963,-1.42365490501938,4.08236976319191));
#10283=CARTESIAN_POINT('Ctrl Pts',(6.48534804172971,-1.42925200704962,4.08184912665446));
#10284=CARTESIAN_POINT('Ctrl Pts',(6.47604534064768,-1.43823666896614,4.08101238754025));
#10285=CARTESIAN_POINT('Ctrl Pts',(6.47248941970006,-1.44164565336273,4.08069467512534));
#10286=CARTESIAN_POINT('Ctrl Pts',(6.46559061582683,-1.44821051806986,4.08008244921019));
#10287=CARTESIAN_POINT('Ctrl Pts',(6.46224942286905,-1.45136804232795,4.07978781585456));
#10288=CARTESIAN_POINT('Ctrl Pts',(6.45420045771056,-1.45892204460257,4.07908245599499));
#10289=CARTESIAN_POINT('Ctrl Pts',(6.44948219682547,-1.4633073721104,4.07867257283375));
#10290=CARTESIAN_POINT('Ctrl Pts',(6.43314007578034,-1.47834946449639,4.07726489955268));
#10291=CARTESIAN_POINT('Ctrl Pts',(6.42141079337622,-1.48889152006443,4.07627531843306));
#10292=CARTESIAN_POINT('Ctrl Pts',(6.35004396862921,-1.5515206630299,4.07036895487261));
#10293=CARTESIAN_POINT('Ctrl Pts',(6.2874667488758,-1.60016386009697,4.06566405075377));
#10294=CARTESIAN_POINT('Ctrl Pts',(6.17740011583619,-1.67566190638798,4.05784717117237));
#10295=CARTESIAN_POINT('Ctrl Pts',(6.13140862784903,-1.70452282664882,4.05470348376064));
#10296=CARTESIAN_POINT('Ctrl Pts',(5.97266525032127,-1.795330209042,4.04408462587772));
#10297=CARTESIAN_POINT('Ctrl Pts',(5.85513409613194,-1.84823520537275,4.03657709673123));
#10298=CARTESIAN_POINT('Ctrl Pts',(5.70989220393536,-1.89739400630095,4.02714428438091));
#10299=CARTESIAN_POINT('Ctrl Pts',(5.68630315111657,-1.90489166883283,4.02560859093979));
#10300=CARTESIAN_POINT('Ctrl Pts',(5.65288771636854,-1.91483188195549,4.02342532564944));
#10301=CARTESIAN_POINT('Ctrl Pts',(5.64317230833253,-1.91764171417169,4.02278962940731));
#10302=CARTESIAN_POINT('Ctrl Pts',(5.62619808557777,-1.92241131926098,4.02167718938542));
#10303=CARTESIAN_POINT('Ctrl Pts',(5.61894871880877,-1.92440417502588,4.02120152256362));
#10304=CARTESIAN_POINT('Ctrl Pts',(5.60373652000043,-1.92849366178767,4.0202021118443));
#10305=CARTESIAN_POINT('Ctrl Pts',(5.59577164076622,-1.93058206091953,4.01967811325639));
#10306=CARTESIAN_POINT('Ctrl Pts',(5.57674034621484,-1.93544635205272,4.01842424269346));
#10307=CARTESIAN_POINT('Ctrl Pts',(5.56566269481705,-1.93817670669019,4.01769292588816));
#10308=CARTESIAN_POINT('Ctrl Pts',(5.52777782491709,-1.94717031191082,4.01518652123842));
#10309=CARTESIAN_POINT('Ctrl Pts',(5.50086564947327,-1.95297336040285,4.01339689600016));
#10310=CARTESIAN_POINT('Ctrl Pts',(5.43574479166177,-1.96561085538815,4.0090423952495));
#10311=CARTESIAN_POINT('Ctrl Pts',(5.39744111586407,-1.97189044755189,4.0064612248424));
#10312=CARTESIAN_POINT('Ctrl Pts',(5.2455210928835,-1.99226532840329,3.99614645484045));
#10313=CARTESIAN_POINT('Ctrl Pts',(5.13097330789122,-1.99768542385434,3.98818313822186));
#10314=CARTESIAN_POINT('Ctrl Pts',(4.91229044824469,-1.98921346808849,3.9729268045579));
#10315=CARTESIAN_POINT('Ctrl Pts',(4.80844168670823,-1.97698892824479,3.96566390672439));
#10316=CARTESIAN_POINT('Ctrl Pts',(4.69003769705261,-1.95352170824858,3.95766231752985));
#10317=CARTESIAN_POINT('Ctrl Pts',(4.67409535379721,-1.95015851834441,3.9565911257986));
#10318=CARTESIAN_POINT('Ctrl Pts',(4.65164316753662,-1.94513391963992,3.95509294647673));
#10319=CARTESIAN_POINT('Ctrl Pts',(4.64509825687946,-1.94363448807067,3.95465747746288));
#10320=CARTESIAN_POINT('Ctrl Pts',(4.6340805167136,-1.94105171695287,3.95392667055196));
#10321=CARTESIAN_POINT('Ctrl Pts',(4.62960367671393,-1.93998590278659,3.95363035383835));
#10322=CARTESIAN_POINT('Ctrl Pts',(4.62044218307069,-1.93777127003361,3.95302531542296));
#10323=CARTESIAN_POINT('Ctrl Pts',(4.61575795031524,-1.93662093950825,3.9527166816312));
#10324=CARTESIAN_POINT('Ctrl Pts',(4.60375933652997,-1.93362819294203,3.95192785812466));
#10325=CARTESIAN_POINT('Ctrl Pts',(4.59645107011538,-1.93176124036041,3.95144905152288));
#10326=CARTESIAN_POINT('Ctrl Pts',(4.56615890249008,-1.9238395684421,3.9494706670552));
#10327=CARTESIAN_POINT('Ctrl Pts',(4.54327248161798,-1.91741548414262,3.94799087193066));
#10328=CARTESIAN_POINT('Ctrl Pts',(4.48229704888695,-1.89911816583587,3.94407497193255));
#10329=CARTESIAN_POINT('Ctrl Pts',(4.44443901521083,-1.88650849878358,3.94167181058319));
#10330=CARTESIAN_POINT('Ctrl Pts',(4.3197300874655,-1.84077110655513,3.93377266870492));
#10331=CARTESIAN_POINT('Ctrl Pts',(4.23481667842238,-1.80271106885129,3.92841814638109));
#10332=CARTESIAN_POINT('Ctrl Pts',(4.03814722745226,-1.6974962820613,3.91545385079092));
#10333=CARTESIAN_POINT('Ctrl Pts',(3.92972636592304,-1.62505898083826,3.90781322595053));
#10334=CARTESIAN_POINT('Ctrl Pts',(3.8166014520879,-1.5323135312837,3.89874153182216));
#10335=CARTESIAN_POINT('Ctrl Pts',(3.8041935596417,-1.52188548189055,3.89773059888617));
#10336=CARTESIAN_POINT('Ctrl Pts',(3.78417475979877,-1.50464032906498,3.89607253990372));
#10337=CARTESIAN_POINT('Ctrl Pts',(3.77648657129276,-1.49791378136283,3.89542911145248));
#10338=CARTESIAN_POINT('Ctrl Pts',(3.76282980752074,-1.48577874924235,3.89427400228424));
#10339=CARTESIAN_POINT('Ctrl Pts',(3.75684164299108,-1.48039257235171,3.8937632565234));
#10340=CARTESIAN_POINT('Ctrl Pts',(3.74421894405368,-1.46889977333143,3.89267746432896));
#10341=CARTESIAN_POINT('Ctrl Pts',(3.73759288562572,-1.46278414994466,3.89210204431425));
#10342=CARTESIAN_POINT('Ctrl Pts',(3.71996612297027,-1.44629253587602,3.89055646449893));
#10343=CARTESIAN_POINT('Ctrl Pts',(3.70904173682172,-1.43583618823217,3.88958288298789));
#10344=CARTESIAN_POINT('Ctrl Pts',(3.65483582539958,-1.38275859321155,3.8846714526289));
#10345=CARTESIAN_POINT('Ctrl Pts',(3.61340224691981,-1.33830421396426,3.88065372563191));
#10346=CARTESIAN_POINT('Ctrl Pts',(3.49097837554367,-1.19430225816004,3.86791789930762));
#10347=CARTESIAN_POINT('Ctrl Pts',(3.41752069534814,-1.08879380085662,3.85894855513481));
#10348=CARTESIAN_POINT('Ctrl Pts',(3.30746079226101,-0.892876529603085,
3.84330737973299));
#10349=CARTESIAN_POINT('Ctrl Pts',(3.26637131767857,-0.805445724567154,
3.83664549145883));
#10350=CARTESIAN_POINT('Ctrl Pts',(3.22784032555064,-0.705152915714656,
3.82958381177159));
#10351=CARTESIAN_POINT('Ctrl Pts',(3.22399716649293,-0.694898056723149,
3.82886835104965));
#10352=CARTESIAN_POINT('Ctrl Pts',(3.21830548518843,-0.679321536867135,
3.827792111869));
#10353=CARTESIAN_POINT('Ctrl Pts',(3.21639480392385,-0.674023036248907,
3.82742784804097));
#10354=CARTESIAN_POINT('Ctrl Pts',(3.21299902101718,-0.664479731489126,
3.82677513562387));
#10355=CARTESIAN_POINT('Ctrl Pts',(3.21150581490721,-0.660237954796991,
3.82648622115841));
#10356=CARTESIAN_POINT('Ctrl Pts',(3.20825677698235,-0.65090773813331,3.82585336244394));
#10357=CARTESIAN_POINT('Ctrl Pts',(3.20650719348742,-0.645817233071268,
3.82550978517489));
#10358=CARTESIAN_POINT('Ctrl Pts',(3.20153464902753,-0.63115656197493,3.82452501337038));
#10359=CARTESIAN_POINT('Ctrl Pts',(3.19836367000329,-0.621568758081545,
3.82388677336884));
#10360=CARTESIAN_POINT('Ctrl Pts',(3.17589339637236,-0.551856025009419,
3.81928516677135));
#10361=CARTESIAN_POINT('Ctrl Pts',(3.15938385495189,-0.490862314019932,
3.81546853706149));
#10362=CARTESIAN_POINT('Ctrl Pts',(3.11767874775922,-0.301565207734443,
3.80397275165978));
#10363=CARTESIAN_POINT('Ctrl Pts',(3.10217018004465,-0.171491505671629,
3.79653640939479));
#10364=CARTESIAN_POINT('Ctrl Pts',(3.0976697843183,0.0483230484799643,3.78360365164448));
#10365=CARTESIAN_POINT('Ctrl Pts',(3.10182483649588,0.137488995768343,3.77826108998273));
#10366=CARTESIAN_POINT('Ctrl Pts',(3.11370470858484,0.241636260315474,3.77175576153798));
#10367=CARTESIAN_POINT('Ctrl Pts',(3.11566344872655,0.257179537500163,3.77077807323617));
#10368=CARTESIAN_POINT('Ctrl Pts',(3.1191791299521,0.282654858790892,3.76916372116944));
#10369=CARTESIAN_POINT('Ctrl Pts',(3.12062845818183,0.292601245675392,3.76853043151641));
#10370=CARTESIAN_POINT('Ctrl Pts',(3.12337200629763,0.310481369968122,3.76738642284655));
#10371=CARTESIAN_POINT('Ctrl Pts',(3.12463913625113,0.318419091580993,3.76687656702241));
#10372=CARTESIAN_POINT('Ctrl Pts',(3.12744628079598,0.335346082279987,3.76578497859009));
#10373=CARTESIAN_POINT('Ctrl Pts',(3.12900003363533,0.344332856328137,3.76520282271844));
#10374=CARTESIAN_POINT('Ctrl Pts',(3.13337713565051,0.368654879339487,3.76362000936851));
#10375=CARTESIAN_POINT('Ctrl Pts',(3.13631871328186,0.383967936436851,3.76261563768816));
#10376=CARTESIAN_POINT('Ctrl Pts',(3.15293405522157,0.465303592599773,3.75723789065463));
#10377=CARTESIAN_POINT('Ctrl Pts',(3.16976768337267,0.530628732653149,3.7527651368445));
#10378=CARTESIAN_POINT('Ctrl Pts',(3.23847015368414,0.750482087264382,3.73717866371862));
#10379=CARTESIAN_POINT('Ctrl Pts',(3.30593618002157,0.899449104254594,3.72563317947668));
#10380=CARTESIAN_POINT('Ctrl Pts',(3.41968622368333,1.08598794387326,3.71063775818693));
#10381=CARTESIAN_POINT('Ctrl Pts',(3.45060167785383,1.13222299687918,3.70687834761051));
#10382=CARTESIAN_POINT('Ctrl Pts',(3.48890050399811,1.18461999645955,3.70261844692349));
#10383=CARTESIAN_POINT('Ctrl Pts',(3.49444233434071,1.19209156297615,3.70201103372938));
#10384=CARTESIAN_POINT('Ctrl Pts',(3.50350488786465,1.20413284879238,3.70103252747815));
#10385=CARTESIAN_POINT('Ctrl Pts',(3.50699344657215,1.20872644328681,3.70065933784227));
#10386=CARTESIAN_POINT('Ctrl Pts',(3.51324231964693,1.21688102855489,3.69999711976966));
#10387=CARTESIAN_POINT('Ctrl Pts',(3.51599481817817,1.22044785945556,3.69970756303625));
#10388=CARTESIAN_POINT('Ctrl Pts',(3.52199718116999,1.22817178588013,3.69908075946758));
#10389=CARTESIAN_POINT('Ctrl Pts',(3.52525146044897,1.23232531998495,3.69874382868134));
#10390=CARTESIAN_POINT('Ctrl Pts',(3.53447341856897,1.24399986427066,3.69779701864955));
#10391=CARTESIAN_POINT('Ctrl Pts',(3.54047906477935,1.25149089368089,3.69718975007611));
#10392=CARTESIAN_POINT('Ctrl Pts',(3.57872284560016,1.29849411340336,3.6933789089183));
#10393=CARTESIAN_POINT('Ctrl Pts',(3.61241507634537,1.33680486857441,3.69027055031326));
#10394=CARTESIAN_POINT('Ctrl Pts',(3.75170794502934,1.48344876530115,3.67816825642467));
#10395=CARTESIAN_POINT('Ctrl Pts',(3.86801266812822,1.58091393616315,3.66962013751421));
#10396=CARTESIAN_POINT('Ctrl Pts',(4.0627695384565,1.7095898487232,3.65584430977834));
#10397=CARTESIAN_POINT('Ctrl Pts',(4.13404099634435,1.75059573212043,3.65090531944602));
#10398=CARTESIAN_POINT('Ctrl Pts',(4.22142951305117,1.79393063080244,3.64484952544176));
#10399=CARTESIAN_POINT('Ctrl Pts',(4.23530570976769,1.8006125794268,3.64388810540857));
#10400=CARTESIAN_POINT('Ctrl Pts',(4.25829045132254,1.81135457392184,3.6422951691027));
#10401=CARTESIAN_POINT('Ctrl Pts',(4.26735470073241,1.81550826277797,3.64166687343972));
#10402=CARTESIAN_POINT('Ctrl Pts',(4.28377595232894,1.8228848339123,3.64052825375207));
#10403=CARTESIAN_POINT('Ctrl Pts',(4.29112204619071,1.82613158723095,3.64001875756983));
#10404=CARTESIAN_POINT('Ctrl Pts',(4.30690215139824,1.83299230544158,3.63892393459924));
#10405=CARTESIAN_POINT('Ctrl Pts',(4.315341866255,1.83659260689268,3.63833815835825));
#10406=CARTESIAN_POINT('Ctrl Pts',(4.33842464417495,1.84625180688925,3.6367352678884));
#10407=CARTESIAN_POINT('Ctrl Pts',(4.35311529890635,1.85219453894624,3.63571427752956));
#10408=CARTESIAN_POINT('Ctrl Pts',(4.43441984209327,1.88396226987241,3.63005769140693));
#10409=CARTESIAN_POINT('Ctrl Pts',(4.50230593188078,1.90636628290309,3.62530992539184));
#10410=CARTESIAN_POINT('Ctrl Pts',(4.76307851271704,1.9771561872093,3.60698129078445));
#10411=CARTESIAN_POINT('Ctrl Pts',(4.96159393700057,2.00026075941747,3.59271506159357));
#10412=CARTESIAN_POINT('Ctrl Pts',(5.18100717846272,1.992952397945,3.57807725593972));
#10413=CARTESIAN_POINT('Ctrl Pts',(5.20177048993695,1.99193572563543,3.57670475659522));
#10414=CARTESIAN_POINT('Ctrl Pts',(5.22991413163123,1.99011629619296,3.57486496418902));
#10415=CARTESIAN_POINT('Ctrl Pts',(5.23731061286233,1.98959670262184,3.57438337592298));
#10416=CARTESIAN_POINT('Ctrl Pts',(5.24901022677738,1.98870923609749,3.57362484649662));
#10417=CARTESIAN_POINT('Ctrl Pts',(5.25331526730577,1.98836861632971,3.57334642906661));
#10418=CARTESIAN_POINT('Ctrl Pts',(5.2622008664577,1.98763653366105,3.57277325673427));
#10419=CARTESIAN_POINT('Ctrl Pts',(5.26678120130415,1.98724321483594,3.57247861914212));
#10420=CARTESIAN_POINT('Ctrl Pts',(5.27777636997539,1.9862607445281,3.57177323029626));
#10421=CARTESIAN_POINT('Ctrl Pts',(5.28418985840642,1.9856563405711,3.57136332256596));
#10422=CARTESIAN_POINT('Ctrl Pts',(5.30629533251938,1.98346504565613,3.56995547363347));
#10423=CARTESIAN_POINT('Ctrl Pts',(5.32197182585846,1.98172307839815,3.56896574418144));
#10424=CARTESIAN_POINT('Ctrl Pts',(5.41623778925947,1.9701148139321,3.56305770284072));
#10425=CARTESIAN_POINT('Ctrl Pts',(5.49421189549902,1.95575966508944,3.5583513995742));
#10426=CARTESIAN_POINT('Ctrl Pts',(5.59267232724365,1.93149505940367,3.55241251324111));
#10427=CARTESIAN_POINT('Ctrl Pts',(5.61412160184396,1.92582797289528,3.55111910548171));
#10428=CARTESIAN_POINT('Ctrl Pts',(5.79247323985027,1.87550864180013,3.54033729976511));
#10429=CARTESIAN_POINT('Ctrl Pts',(5.94342959345671,1.81212826871002,3.53097196477376));
#10430=CARTESIAN_POINT('Ctrl Pts',(6.10509183627556,1.71956631779482,3.51949302039675));
#10431=CARTESIAN_POINT('Ctrl Pts',(6.12499941118154,1.70770263392336,3.51805349302589));
#10432=CARTESIAN_POINT('Ctrl Pts',(6.15379969465358,1.6898522166908,3.51593031143604));
#10433=CARTESIAN_POINT('Ctrl Pts',(6.16285847219723,1.68413607965307,3.51525649647807));
#10434=CARTESIAN_POINT('Ctrl Pts',(6.17861062085973,1.67401808998066,3.51407406421678));
#10435=CARTESIAN_POINT('Ctrl Pts',(6.18532438700091,1.66964832311669,3.51356663997991));
#10436=CARTESIAN_POINT('Ctrl Pts',(6.19828736545144,1.66109955202571,3.51258008721594));
#10437=CARTESIAN_POINT('Ctrl Pts',(6.20453964092166,1.65692542055978,3.51210114654019));
#10438=CARTESIAN_POINT('Ctrl Pts',(6.22092866919317,1.64584936409896,3.51083740566849));
#10439=CARTESIAN_POINT('Ctrl Pts',(6.23102550445284,1.63888921392634,3.51005042298985));
#10440=CARTESIAN_POINT('Ctrl Pts',(6.26818543475536,1.61276466483037,3.50712219344519));
#10441=CARTESIAN_POINT('Ctrl Pts',(6.29483228988954,1.59302030171959,3.5049589910087));
#10442=CARTESIAN_POINT('Ctrl Pts',(6.36022367553467,1.54199418225084,3.49948585862434));
#10443=CARTESIAN_POINT('Ctrl Pts',(6.3983106728703,1.50991002685388,3.49614642308244));
#10444=CARTESIAN_POINT('Ctrl Pts',(6.51607246560829,1.40292462004297,3.48533020141262));
#10445=CARTESIAN_POINT('Ctrl Pts',(6.59080392461046,1.32288934194362,3.47768858874758));
#10446=CARTESIAN_POINT('Ctrl Pts',(6.72001423243646,1.15946105250098,3.46318190124743));
#10447=CARTESIAN_POINT('Ctrl Pts',(6.77556957581477,1.07730282279316,3.45633483650199));
#10448=CARTESIAN_POINT('Ctrl Pts',(6.83024285758485,0.981839176404877,3.44910403192548));
#10449=CARTESIAN_POINT('Ctrl Pts',(6.83561086552789,0.972284515571788,3.44838804159841));
#10450=CARTESIAN_POINT('Ctrl Pts',(6.84361906219759,0.957751318688625,3.44731116621229));
#10451=CARTESIAN_POINT('Ctrl Pts',(6.84631724651666,0.952805220369281,3.44694678979151));
#10452=CARTESIAN_POINT('Ctrl Pts',(6.8511313235749,0.943890802064821,3.44629395944234));
#10453=CARTESIAN_POINT('Ctrl Pts',(6.85325477585697,0.939926718030011,3.44600503884596));
#10454=CARTESIAN_POINT('Ctrl Pts',(6.8578897959809,0.931203264826867,3.44537226539275));
#10455=CARTESIAN_POINT('Ctrl Pts',(6.86039551493203,0.926440906401836,3.4450287788303));
#10456=CARTESIAN_POINT('Ctrl Pts',(6.86754463320332,0.91271885399775,3.44404452895397));
#10457=CARTESIAN_POINT('Ctrl Pts',(6.87213943539684,0.903733833824589,3.44340671531134));
#10458=CARTESIAN_POINT('Ctrl Pts',(6.90490003060749,0.83845391932637,3.43881795304588));
#10459=CARTESIAN_POINT('Ctrl Pts',(6.93045833880855,0.780882535163358,3.43501281075605));
#10460=CARTESIAN_POINT('Ctrl Pts',(7.00707875344604,0.583608389057448,3.42246005125068));
#10461=CARTESIAN_POINT('Ctrl Pts',(7.04524375895339,0.439439501650824,3.41404333454195));
#10462=CARTESIAN_POINT('Ctrl Pts',(7.0772801406051,0.223220693816843,3.40107997807778));
#10463=CARTESIAN_POINT('Ctrl Pts',(7.08388258814698,0.15359383560584,3.3968617862632));
#10464=CARTESIAN_POINT('Ctrl Pts',(7.0875124804748,0.0672331879277639,3.39150336582134));
#10465=CARTESIAN_POINT('Ctrl Pts',(7.08800166959783,0.050689824531779,3.39047131458294));
#10466=CARTESIAN_POINT('Ctrl Pts',(7.08840915873896,0.026886180326674,3.38897753977713));
#10467=CARTESIAN_POINT('Ctrl Pts',(7.08849377643241,0.0196291480183904,
3.38852095762822));
#10468=CARTESIAN_POINT('Ctrl Pts',(7.08856446090382,0.00823273870908804,
3.3878020387734));
#10469=CARTESIAN_POINT('Ctrl Pts',(7.08857724960592,0.00409354651653826,
3.38754053199994));
#10470=CARTESIAN_POINT('Ctrl Pts',(7.08857715493132,-4.56255882934932E-5,
3.38727862543405));
#10471=CARTESIAN_POINT('Ctrl Pts',(7.08857715545311,9.38937122496597E-11,
3.22796126976449));
#10472=CARTESIAN_POINT('Ctrl Pts',(7.08857715544517,0.168685454855076,3.2377853965787));
#10473=CARTESIAN_POINT('Ctrl Pts',(7.06718218800094,0.336672451181935,3.24744467620048));
#10474=CARTESIAN_POINT('Ctrl Pts',(7.01913649848504,0.522246460643926,3.25926483344194));
#10475=CARTESIAN_POINT('Ctrl Pts',(7.01298196209565,0.544428316921216,3.26069567714573));
#10476=CARTESIAN_POINT('Ctrl Pts',(7.00345982108771,0.576577093536144,3.26279790899861));
#10477=CARTESIAN_POINT('Ctrl Pts',(7.00039492230318,0.586632257973225,3.26345951558006));
#10478=CARTESIAN_POINT('Ctrl Pts',(6.99482333860884,0.604406263268823,3.26463647925897));
#10479=CARTESIAN_POINT('Ctrl Pts',(6.99234873670921,0.612134970242019,3.26515078099188));
#10480=CARTESIAN_POINT('Ctrl Pts',(6.98710057930681,0.628188102074734,3.2662243793466));
#10481=CARTESIAN_POINT('Ctrl Pts',(6.98431912661748,0.636509742253686,3.2667839255307));
#10482=CARTESIAN_POINT('Ctrl Pts',(6.97695220991413,0.658076010461559,3.26824201714204));
#10483=CARTESIAN_POINT('Ctrl Pts',(6.97228195603154,0.671290959196758,3.2691433357174));
#10484=CARTESIAN_POINT('Ctrl Pts',(6.95101155575453,0.729517105215765,3.27315025192122));
#10485=CARTESIAN_POINT('Ctrl Pts',(6.93293121296876,0.773966872729414,3.27630442957034));
#10486=CARTESIAN_POINT('Ctrl Pts',(6.87841998155473,0.895255431543577,3.28518496806801));
#10487=CARTESIAN_POINT('Ctrl Pts',(6.83865528022506,0.970477159813528,3.29101165325064));
#10488=CARTESIAN_POINT('Ctrl Pts',(6.72375800552674,1.15780610754,3.306262611492));
#10489=CARTESIAN_POINT('Ctrl Pts',(6.64183493106537,1.26525275239806,3.31577328896848));
#10490=CARTESIAN_POINT('Ctrl Pts',(6.53240299116342,1.38208804644868,3.32650198171037));
#10491=CARTESIAN_POINT('Ctrl Pts',(6.51475495195988,1.4002257470951,3.32817912157778));
#10492=CARTESIAN_POINT('Ctrl Pts',(6.49107378136203,1.4236549923912,3.3303553238341));
#10493=CARTESIAN_POINT('Ctrl Pts',(6.48534797027268,1.42925207647901,3.33087595870867));
#10494=CARTESIAN_POINT('Ctrl Pts',(6.47604529059742,1.43823671704978,3.33171269584108));
#10495=CARTESIAN_POINT('Ctrl Pts',(6.47248937315868,1.44164569785363,3.33203040792309));
#10496=CARTESIAN_POINT('Ctrl Pts',(6.46559057005701,1.44821056143531,3.33264263373642));
#10497=CARTESIAN_POINT('Ctrl Pts',(6.46224937431774,1.45136808811623,3.33293726731979));
#10498=CARTESIAN_POINT('Ctrl Pts',(6.4542003936161,1.45892210444373,3.33364262849662));
#10499=CARTESIAN_POINT('Ctrl Pts',(6.44948211987209,1.46330744347849,3.33405251273967));
#10500=CARTESIAN_POINT('Ctrl Pts',(6.43313991047296,1.47834961534023,3.3354601934806));
#10501=CARTESIAN_POINT('Ctrl Pts',(6.42141055106612,1.48889173719833,3.33644978086266));
#10502=CARTESIAN_POINT('Ctrl Pts',(6.35004285449729,1.55152161820794,3.34235621452919));
#10503=CARTESIAN_POINT('Ctrl Pts',(6.28746476248122,1.60016539335824,3.34706117706064));
#10504=CARTESIAN_POINT('Ctrl Pts',(6.17741057557539,1.67565461476364,3.35487715953641));
#10505=CARTESIAN_POINT('Ctrl Pts',(6.13143321066452,1.70450734343938,3.35801991298445));
#10506=CARTESIAN_POINT('Ctrl Pts',(5.97269202358152,1.79531825991671,3.36863875155969));
#10507=CARTESIAN_POINT('Ctrl Pts',(5.85514660269822,1.84823117735319,3.37614716843463));
#10508=CARTESIAN_POINT('Ctrl Pts',(5.70988998249731,1.89739471872135,3.38558093914143));
#10509=CARTESIAN_POINT('Ctrl Pts',(5.68630156940592,1.90489215196905,3.38711659121429));
#10510=CARTESIAN_POINT('Ctrl Pts',(5.65288689141644,1.91483212219995,3.38929980726434));
#10511=CARTESIAN_POINT('Ctrl Pts',(5.64317159339087,1.91764191837016,3.38993549636044));
#10512=CARTESIAN_POINT('Ctrl Pts',(5.62619750690776,1.92241147940399,3.3910479275253));
#10513=CARTESIAN_POINT('Ctrl Pts',(5.61894816599453,1.92440432576779,3.39152359268106));
#10514=CARTESIAN_POINT('Ctrl Pts',(5.6037359661584,1.92849380834459,3.39252300352889));
#10515=CARTESIAN_POINT('Ctrl Pts',(5.59577105987582,1.93058221206542,3.39304700393154));
#10516=CARTESIAN_POINT('Ctrl Pts',(5.57673959783384,1.93544653962978,3.39430088562208));
#10517=CARTESIAN_POINT('Ctrl Pts',(5.56566180549297,1.93817692403709,3.39503221180626));
#10518=CARTESIAN_POINT('Ctrl Pts',(5.52777593983032,1.94717074438924,3.39753868266361));
#10519=CARTESIAN_POINT('Ctrl Pts',(5.50086290237092,1.95297394527661,3.39932836576618));
#10520=CARTESIAN_POINT('Ctrl Pts',(5.43573957227161,1.96561179528322,3.4036830339539));
#10521=CARTESIAN_POINT('Ctrl Pts',(5.397434277516,1.9718915323255,3.40626431558079));
#10522=CARTESIAN_POINT('Ctrl Pts',(5.24550388666742,1.99226714138722,3.41657980066685));
#10523=CARTESIAN_POINT('Ctrl Pts',(5.13094725159728,1.99768640957115,3.42454375649992));
#10524=CARTESIAN_POINT('Ctrl Pts',(4.91226739539063,1.98921075493262,3.43979988447141));
#10525=CARTESIAN_POINT('Ctrl Pts',(4.80843032309346,1.97698667467482,3.44706194007859));
#10526=CARTESIAN_POINT('Ctrl Pts',(4.69003771629629,1.95352171227245,3.45506276007776));
#10527=CARTESIAN_POINT('Ctrl Pts',(4.67409536758635,1.95015852135857,3.45613395218003));
#10528=CARTESIAN_POINT('Ctrl Pts',(4.65164317429171,1.9451339211812,3.45763213197464));
#10529=CARTESIAN_POINT('Ctrl Pts',(4.64509826203054,1.94363448926557,3.45806760109595));
#10530=CARTESIAN_POINT('Ctrl Pts',(4.63408051936311,1.94105171758261,3.45879840817356));
#10531=CARTESIAN_POINT('Ctrl Pts',(4.62960367846387,1.93998590320752,3.45909472494692));
#10532=CARTESIAN_POINT('Ctrl Pts',(4.62044218313054,1.93777127005026,3.4596997634741));
#10533=CARTESIAN_POINT('Ctrl Pts',(4.61575794958448,1.93662093932988,3.46000839731793));
#10534=CARTESIAN_POINT('Ctrl Pts',(4.60375933397472,1.93362819229858,3.46079722094412));
#10535=CARTESIAN_POINT('Ctrl Pts',(4.59645106652795,1.93176123944092,3.46127602761315));
#10536=CARTESIAN_POINT('Ctrl Pts',(4.56615889609478,1.9238395667109,3.46325441226205));
#10537=CARTESIAN_POINT('Ctrl Pts',(4.54327247346199,1.91741548182374,3.46473420749827));
#10538=CARTESIAN_POINT('Ctrl Pts',(4.48229703683551,1.89911816200378,3.46865010774123));
#10539=CARTESIAN_POINT('Ctrl Pts',(4.44443900105115,1.88650849395834,3.47105326922216));
#10540=CARTESIAN_POINT('Ctrl Pts',(4.31973007500538,1.84077110112843,3.47895241099657));
#10541=CARTESIAN_POINT('Ctrl Pts',(4.23481666957667,1.80271106444529,3.4843069331157));
#10542=CARTESIAN_POINT('Ctrl Pts',(4.03814722747321,1.69749628161576,3.49727122816487));
#10543=CARTESIAN_POINT('Ctrl Pts',(3.92972637085183,1.62505898389022,3.50491185266703));
#10544=CARTESIAN_POINT('Ctrl Pts',(3.81660145956486,1.53231353753691,3.5139835465249));
#10545=CARTESIAN_POINT('Ctrl Pts',(3.80419356555638,1.52188548692369,3.51499447958252));
#10546=CARTESIAN_POINT('Ctrl Pts',(3.78417476297861,1.50464033184335,3.51665253878526));
#10547=CARTESIAN_POINT('Ctrl Pts',(3.77648657328467,1.49791378312528,3.51729596733447));
#10548=CARTESIAN_POINT('Ctrl Pts',(3.76282980725424,1.48577874901147,3.51845107669293));
#10549=CARTESIAN_POINT('Ctrl Pts',(3.75684164164996,1.48039257114839,3.51896182254581));
#10550=CARTESIAN_POINT('Ctrl Pts',(3.74421894028102,1.4688997698766,3.52004761495186));
#10551=CARTESIAN_POINT('Ctrl Pts',(3.73759288050139,1.46278414520507,3.52062303508637));
#10552=CARTESIAN_POINT('Ctrl Pts',(3.71996611381691,1.44629252722031,3.52216861526454));
#10553=CARTESIAN_POINT('Ctrl Pts',(3.70904172503282,1.43583617690194,3.52314219702043));
#10554=CARTESIAN_POINT('Ctrl Pts',(3.65483579272347,1.38275856035883,3.52805362934279));
#10555=CARTESIAN_POINT('Ctrl Pts',(3.61340219766025,1.33830416066351,3.53207135812795));
#10556=CARTESIAN_POINT('Ctrl Pts',(3.49097824925787,1.19430209981282,3.54480719343686));
#10557=CARTESIAN_POINT('Ctrl Pts',(3.41752052282418,1.08879354745196,3.55377654524543));
#10558=CARTESIAN_POINT('Ctrl Pts',(3.30746067700814,0.892876284046156,3.56941771786359));
#10559=CARTESIAN_POINT('Ctrl Pts',(3.26637127044077,0.805445600785516,3.57607959613874));
#10560=CARTESIAN_POINT('Ctrl Pts',(3.22784032729168,0.705152920340156,3.58314126680652));
#10561=CARTESIAN_POINT('Ctrl Pts',(3.22399716779749,0.694898060252058,3.58385672760659));
#10562=CARTESIAN_POINT('Ctrl Pts',(3.21830548577588,0.67932153849607,3.58493296692));
#10563=CARTESIAN_POINT('Ctrl Pts',(3.21639480421915,0.674023037078554,3.58529723080324));
#10564=CARTESIAN_POINT('Ctrl Pts',(3.21299902075027,0.664479730739243,3.58594994332835));
#10565=CARTESIAN_POINT('Ctrl Pts',(3.21150581436864,0.660237953267188,3.58623885784671));
#10566=CARTESIAN_POINT('Ctrl Pts',(3.20825677578016,0.650907734660911,3.58687171669202));
#10567=CARTESIAN_POINT('Ctrl Pts',(3.20650719189738,0.645817228434815,3.58721529403877));
#10568=CARTESIAN_POINT('Ctrl Pts',(3.20153464612462,0.631156553319627,3.58820006610978));
#10569=CARTESIAN_POINT('Ctrl Pts',(3.19836366620917,0.621568746560217,3.58883830629828));
#10570=CARTESIAN_POINT('Ctrl Pts',(3.17589337706522,0.551855963548858,3.59343991615476));
#10571=CARTESIAN_POINT('Ctrl Pts',(3.15938382546428,0.490862204156248,3.59725654871097));
#10572=CARTESIAN_POINT('Ctrl Pts',(3.11767866472496,0.301564781234179,3.60875235275822));
#10573=CARTESIAN_POINT('Ctrl Pts',(3.10217010175756,0.171490803308188,3.61618870989906));
#10574=CARTESIAN_POINT('Ctrl Pts',(3.09766981425869,-0.0483237159697841,
3.62912146723118));
#10575=CARTESIAN_POINT('Ctrl Pts',(3.1018248749594,-0.137489353042398,3.63446401120191));
#10576=CARTESIAN_POINT('Ctrl Pts',(3.11370471374329,-0.241636302010408,
3.64096932003552));
#10577=CARTESIAN_POINT('Ctrl Pts',(3.11566345306548,-0.257179570332415,
3.6419470077915));
#10578=CARTESIAN_POINT('Ctrl Pts',(3.11917913314574,-0.282654881039812,
3.64356135920014));
#10579=CARTESIAN_POINT('Ctrl Pts',(3.12062846123137,-0.292601266180397,
3.64419464874659));
#10580=CARTESIAN_POINT('Ctrl Pts',(3.12337200942936,-0.310481389873712,
3.64533865738518));
#10581=CARTESIAN_POINT('Ctrl Pts',(3.12463913964924,-0.31841911262524,3.64584851328592));
#10582=CARTESIAN_POINT('Ctrl Pts',(3.12744628524539,-0.335346108481486,
3.64694010205887));
#10583=CARTESIAN_POINT('Ctrl Pts',(3.12900003891108,-0.344332886540949,
3.64752225819586));
#10584=CARTESIAN_POINT('Ctrl Pts',(3.13337714454712,-0.368654927240598,
3.64910507271514));
#10585=CARTESIAN_POINT('Ctrl Pts',(3.1363187252391,-0.383967997962829,3.65010944530784));
#10586=CARTESIAN_POINT('Ctrl Pts',(3.15293410991627,-0.465303847400993,
3.65548720525991));
#10587=CARTESIAN_POINT('Ctrl Pts',(3.16976779559368,-0.530629162928124,
3.65995997164014));
#10588=CARTESIAN_POINT('Ctrl Pts',(3.23847074818011,-0.750483817708959,
3.6755465402418));
#10589=CARTESIAN_POINT('Ctrl Pts',(3.30593745665356,-0.899451859374783,
3.68709211468425));
#10590=CARTESIAN_POINT('Ctrl Pts',(3.41968783916793,-1.08599036734191,3.70208751766366));
#10591=CARTESIAN_POINT('Ctrl Pts',(3.45060261776856,-1.13222429677065,3.70584683697757));
#10592=CARTESIAN_POINT('Ctrl Pts',(3.48890064838236,-1.18462019165321,3.71010664784652));
#10593=CARTESIAN_POINT('Ctrl Pts',(3.49444244778048,-1.1920917147581,3.71071405750844));
#10594=CARTESIAN_POINT('Ctrl Pts',(3.50350496079102,-1.20413294503375,3.71169255924212));
#10595=CARTESIAN_POINT('Ctrl Pts',(3.50699351042237,-1.20872652703664,3.71206574786143));
#10596=CARTESIAN_POINT('Ctrl Pts',(3.51324237418476,-1.21688109939131,3.71272796488251));
#10597=CARTESIAN_POINT('Ctrl Pts',(3.51599487258273,-1.22044792978967,3.7130175215736));
#10598=CARTESIAN_POINT('Ctrl Pts',(3.52199724358281,-1.22817186581259,3.71364432591847));
#10599=CARTESIAN_POINT('Ctrl Pts',(3.52525153108682,-1.23232540995246,3.71398125751727));
#10600=CARTESIAN_POINT('Ctrl Pts',(3.53447353362177,-1.24400000893292,3.71492807198143));
#10601=CARTESIAN_POINT('Ctrl Pts',(3.54047921659056,-1.25149108254966,3.7155353441363));
#10602=CARTESIAN_POINT('Ctrl Pts',(3.57872377603487,-1.29849524480288,3.71934626172196));
#10603=CARTESIAN_POINT('Ctrl Pts',(3.61241681643663,-1.33680684136023,3.72245468876477));
#10604=CARTESIAN_POINT('Ctrl Pts',(3.75171710117433,-1.48345798689375,3.73455759135895));
#10605=CARTESIAN_POINT('Ctrl Pts',(3.86802979852114,-1.58092809878593,3.74310620313579));
#10606=CARTESIAN_POINT('Ctrl Pts',(4.06278830165982,-1.70960070047408,3.75688206918397));
#10607=CARTESIAN_POINT('Ctrl Pts',(4.13405170903037,-1.7506011522757,3.76182050195941));
#10608=CARTESIAN_POINT('Ctrl Pts',(4.22143126178332,-1.79393147774978,3.76787567467788));
#10609=CARTESIAN_POINT('Ctrl Pts',(4.23530710024496,-1.80061323894182,3.76883706989948));
#10610=CARTESIAN_POINT('Ctrl Pts',(4.25829137088769,-1.81135499742174,3.77042997358977));
#10611=CARTESIAN_POINT('Ctrl Pts',(4.26735551090812,-1.8155086309207,3.77105826168098));
#10612=CARTESIAN_POINT('Ctrl Pts',(4.28377664625156,-1.82288514224108,3.77219687332661));
#10613=CARTESIAN_POINT('Ctrl Pts',(4.29112273397342,-1.82613188952116,3.77270636909272));
#10614=CARTESIAN_POINT('Ctrl Pts',(4.30690291655853,-1.83299263438238,3.77380119745486));
#10615=CARTESIAN_POINT('Ctrl Pts',(4.31534271545483,-1.83659296729466,3.77438697954499));
#10616=CARTESIAN_POINT('Ctrl Pts',(4.33842595595339,-1.84625234709807,3.77598990219368));
#10617=CARTESIAN_POINT('Ctrl Pts',(4.3531169923676,-1.85219521965553,3.77701091914311));
#10618=CARTESIAN_POINT('Ctrl Pts',(4.4344281634835,-1.88396543543093,3.78266796694263));
#10619=CARTESIAN_POINT('Ctrl Pts',(4.5023207381432,-1.90637112691631,3.78741618992693));
#10620=CARTESIAN_POINT('Ctrl Pts',(4.76318759513982,-1.97718350268646,3.80575146708481));
#10621=CARTESIAN_POINT('Ctrl Pts',(4.96179591185586,-2.00028306631814,3.82002462665903));
#10622=CARTESIAN_POINT('Ctrl Pts',(5.18122283748945,-1.99294216699515,3.83466209118415));
#10623=CARTESIAN_POINT('Ctrl Pts',(5.20191068399526,-1.9919273374996,3.83602951847649));
#10624=CARTESIAN_POINT('Ctrl Pts',(5.2299686486106,-1.99011252900006,3.83786366725163));
#10625=CARTESIAN_POINT('Ctrl Pts',(5.23735480239263,-1.98959347681001,3.83834457417821));
#10626=CARTESIAN_POINT('Ctrl Pts',(5.24904206210842,-1.98870674724812,3.83910229275337));
#10627=CARTESIAN_POINT('Ctrl Pts',(5.25334506921535,-1.9883662212601,3.83938057530421));
#10628=CARTESIAN_POINT('Ctrl Pts',(5.26222994919408,-1.98763407289399,3.83995369487418));
#10629=CARTESIAN_POINT('Ctrl Pts',(5.26681159701087,-1.98724057226022,3.84024841340139));
#10630=CARTESIAN_POINT('Ctrl Pts',(5.27781551482398,-1.98625714316381,3.84095435480886));
#10631=CARTESIAN_POINT('Ctrl Pts',(5.28423643385009,-1.98565189915354,3.84136473072139));
#10632=CARTESIAN_POINT('Ctrl Pts',(5.30639495046331,-1.98345473748275,3.84277592973379));
#10633=CARTESIAN_POINT('Ctrl Pts',(5.32211694904346,-1.98170673159543,3.84376848854349));
#10634=CARTESIAN_POINT('Ctrl Pts',(5.41690021275341,-1.97002550684214,3.84970859685526));
#10635=CARTESIAN_POINT('Ctrl Pts',(5.4953376592896,-1.95554822630603,3.85444163959602));
#10636=CARTESIAN_POINT('Ctrl Pts',(5.58586114571642,-1.93316159423466,3.85990172187665));
#10637=CARTESIAN_POINT('Ctrl Pts',(5.59898264065211,-1.92977437499375,3.86069306372408));
#10638=CARTESIAN_POINT('Ctrl Pts',(5.77900740569764,-1.88134030198174,3.87156010179077));
#10639=CARTESIAN_POINT('Ctrl Pts',(5.93938070271494,-1.81492346102197,3.88143896606319));
#10640=CARTESIAN_POINT('Ctrl Pts',(6.10835299924791,-1.71763041237996,3.8934674576784));
#10641=CARTESIAN_POINT('Ctrl Pts',(6.12733808787899,-1.70627430781312,3.89484274368384));
#10642=CARTESIAN_POINT('Ctrl Pts',(6.15505287621803,-1.68906419510839,3.89688782061571));
#10643=CARTESIAN_POINT('Ctrl Pts',(6.1639318823387,-1.68345292549688,3.89754877663661));
#10644=CARTESIAN_POINT('Ctrl Pts',(6.17947418317278,-1.67345800741364,3.8987161631305));
#10645=CARTESIAN_POINT('Ctrl Pts',(6.18615632842068,-1.66910399503938,3.89922149054561));
#10646=CARTESIAN_POINT('Ctrl Pts',(6.19908220481033,-1.66057077126476,3.90020576446135));
#10647=CARTESIAN_POINT('Ctrl Pts',(6.20532879698651,-1.65639612075254,3.90068453472512));
#10648=CARTESIAN_POINT('Ctrl Pts',(6.22191913656929,-1.64517255136957,3.90196450605855));
#10649=CARTESIAN_POINT('Ctrl Pts',(6.23222023851879,-1.63806148183562,3.90276803785077));
#10650=CARTESIAN_POINT('Ctrl Pts',(6.27107327470375,-1.6106969104163,3.90583279846002));
#10651=CARTESIAN_POINT('Ctrl Pts',(6.2991558376273,-1.5897910160843,3.90811873547069));
#10652=CARTESIAN_POINT('Ctrl Pts',(6.36883122861123,-1.5350140298848,3.9139764836569));
#10653=CARTESIAN_POINT('Ctrl Pts',(6.40963297870938,-1.50018587978312,3.91758339883017));
#10654=CARTESIAN_POINT('Ctrl Pts',(6.51495750668446,-1.40267611630217,3.92737147528454));
#10655=CARTESIAN_POINT('Ctrl Pts',(6.57672621637369,-1.33720609366694,3.9336360307158));
#10656=CARTESIAN_POINT('Ctrl Pts',(6.69998997885088,-1.1874734670786,3.94715606273761));
#10657=CARTESIAN_POINT('Ctrl Pts',(6.75973657549667,-1.10208997928839,3.95439336778145));
#10658=CARTESIAN_POINT('Ctrl Pts',(6.82082241454186,-0.998388902066491,
3.96237164322743));
#10659=CARTESIAN_POINT('Ctrl Pts',(6.82891987929916,-0.984249107201606,
3.96344290339751));
#10660=CARTESIAN_POINT('Ctrl Pts',(6.84010861807734,-0.964144024554281,
3.96494116119756));
#10661=CARTESIAN_POINT('Ctrl Pts',(6.84334416331121,-0.958260345174318,
3.96537664141484));
#10662=CARTESIAN_POINT('Ctrl Pts',(6.84874709657984,-0.9483167931981,3.96610746168287));
#10663=CARTESIAN_POINT('Ctrl Pts',(6.85093023728254,-0.944265588357725,
3.96640378062932));
#10664=CARTESIAN_POINT('Ctrl Pts',(6.85537278959444,-0.93595288632395,3.96700881824968));
#10665=CARTESIAN_POINT('Ctrl Pts',(6.85763079299438,-0.931690697589313,
3.96731744904535));
#10666=CARTESIAN_POINT('Ctrl Pts',(6.86338009900063,-0.920742543993711,
3.96810625556856));
#10667=CARTESIAN_POINT('Ctrl Pts',(6.86684901822192,-0.914044818825352,
3.96858504829917));
#10668=CARTESIAN_POINT('Ctrl Pts',(6.88109002063351,-0.886162417382578,
3.970563298827));
#10669=CARTESIAN_POINT('Ctrl Pts',(6.8915215668731,-0.864804775530169,3.9720429772356));
#10670=CARTESIAN_POINT('Ctrl Pts',(6.91843124332041,-0.807117362150341,
3.97595848727869));
#10671=CARTESIAN_POINT('Ctrl Pts',(6.93420612063805,-0.77047009790331,3.97836138347411));
#10672=CARTESIAN_POINT('Ctrl Pts',(7.00351062640271,-0.595166244652166,
3.98957139501167));
#10673=CARTESIAN_POINT('Ctrl Pts',(7.04253450382315,-0.451284364024468,
3.99798163952158));
#10674=CARTESIAN_POINT('Ctrl Pts',(7.07639767614088,-0.231973801152632,
4.01111595482023));
#10675=CARTESIAN_POINT('Ctrl Pts',(7.08357992194477,-0.158996585193538,
4.01553010832341));
#10676=CARTESIAN_POINT('Ctrl Pts',(7.08746223093588,-0.0688155482614963,
4.02112309351378));
#10677=CARTESIAN_POINT('Ctrl Pts',(7.08797615278786,-0.051828010141138,
4.0221825172722));
#10678=CARTESIAN_POINT('Ctrl Pts',(7.08840213305802,-0.027439866292334,
4.02371272051326));
#10679=CARTESIAN_POINT('Ctrl Pts',(7.08849017770342,-0.0200427758340486,
4.02417806009595));
#10680=CARTESIAN_POINT('Ctrl Pts',(7.08856389118241,-0.00841511051592803,
4.02491151845259));
#10681=CARTESIAN_POINT('Ctrl Pts',(7.08857725168938,-0.00418473261553051,
4.02517877714476));
#10682=CARTESIAN_POINT('Ctrl Pts',(7.08857715493134,4.56245408300607E-5,
4.02544645345466));
#10683=CARTESIAN_POINT('Origin',(5.09382715545311,0.,-6.77268258743872));
#10684=CARTESIAN_POINT('',(7.08857715545311,-3.14645820945244E-12,4.98428615635939));
#10685=CARTESIAN_POINT('',(7.08857715545311,4.63564351804039E-12,4.82758772788682));
#10686=CARTESIAN_POINT('',(7.08857715545311,8.3550772080578E-14,-6.77268258743872));
#10687=CARTESIAN_POINT('',(7.08857712267089,-0.00123466680453736,4.98420171859293));
#10688=CARTESIAN_POINT('Ctrl Pts',(7.08857715545311,-3.14645820945244E-12,
4.98428615635939));
#10689=CARTESIAN_POINT('Ctrl Pts',(7.08857715545311,-0.000410617569554449,
4.98425787060343));
#10690=CARTESIAN_POINT('Ctrl Pts',(7.0885770286652,-0.000821238879055287,
4.9842295872048));
#10691=CARTESIAN_POINT('Ctrl Pts',(7.08857677508245,-0.00123186387362816,
4.98420130618351));
#10692=CARTESIAN_POINT('Ctrl Pts',(7.08857677337535,-0.0012346250781053,
4.9842011160108));
#10693=CARTESIAN_POINT('Ctrl Pts',(7.08854025461787,-0.0602369722889442,
4.98013744242997));
#10694=CARTESIAN_POINT('Ctrl Pts',(7.08588590358347,-0.119215683551362,
4.97612891140116));
#10695=CARTESIAN_POINT('Ctrl Pts',(7.07982904051931,-0.186822383758213,
4.97165554826758));
#10696=CARTESIAN_POINT('Ctrl Pts',(7.07897947543163,-0.195643460673842,
4.97107428786379));
#10697=CARTESIAN_POINT('Ctrl Pts',(7.07749276312789,-0.210071797355168,
4.97012779847945));
#10698=CARTESIAN_POINT('Ctrl Pts',(7.07689056722123,-0.215682428229593,
4.96976080043087));
#10699=CARTESIAN_POINT('Ctrl Pts',(7.07577889558268,-0.225641370710706,
4.96911133905215));
#10700=CARTESIAN_POINT('Ctrl Pts',(7.07527890089432,-0.229990673185066,
4.96882837042057));
#10701=CARTESIAN_POINT('Ctrl Pts',(7.07423564991491,-0.238809609413973,
4.96825600445741));
#10702=CARTESIAN_POINT('Ctrl Pts',(7.07369157716984,-0.243279073122874,
4.96796666377202));
#10703=CARTESIAN_POINT('Ctrl Pts',(7.0724734288636,-0.253011135418825,4.96733825137212));
#10704=CARTESIAN_POINT('Ctrl Pts',(7.07179349057742,-0.258272895622735,
4.96699950973492));
#10705=CARTESIAN_POINT('Ctrl Pts',(7.06984161671701,-0.27291769523819,4.96605938464704));
#10706=CARTESIAN_POINT('Ctrl Pts',(7.06852383336751,-0.282294629957024,
4.96546049546868));
#10707=CARTESIAN_POINT('Ctrl Pts',(7.06090677739358,-0.333829717906222,
4.96218415431966));
#10708=CARTESIAN_POINT('Ctrl Pts',(7.05332371500427,-0.375790295018537,
4.95957219553235));
#10709=CARTESIAN_POINT('Ctrl Pts',(7.0361789592161,-0.45589522114539,4.95463801597854));
#10710=CARTESIAN_POINT('Ctrl Pts',(7.02682326220819,-0.494062050879139,
4.95231024669574));
#10711=CARTESIAN_POINT('Ctrl Pts',(6.97721082332847,-0.67337321319461,4.94138270652834));
#10712=CARTESIAN_POINT('Ctrl Pts',(6.92258770274573,-0.810062229424848,
4.93304200405361));
#10713=CARTESIAN_POINT('Ctrl Pts',(6.82543272284463,-0.992024066641868,
4.92070027154727));
#10714=CARTESIAN_POINT('Ctrl Pts',(6.79506813422487,-1.04323904280439,4.91707890843787));
#10715=CARTESIAN_POINT('Ctrl Pts',(6.75422723196292,-1.105588074991,4.91243889070054));
#10716=CARTESIAN_POINT('Ctrl Pts',(6.74585102741146,-1.11806552254119,4.91149827621661));
#10717=CARTESIAN_POINT('Ctrl Pts',(6.73223646878752,-1.13785913859887,4.90998613732503));
#10718=CARTESIAN_POINT('Ctrl Pts',(6.7270881048697,-1.14523672843157,4.909418008423));
#10719=CARTESIAN_POINT('Ctrl Pts',(6.71723414447937,-1.15915583120775,4.90833740366725));
#10720=CARTESIAN_POINT('Ctrl Pts',(6.71253845968714,-1.16570416636264,4.90782531319366));
#10721=CARTESIAN_POINT('Ctrl Pts',(6.70177949998019,-1.18051763818208,4.90665830471736));
#10722=CARTESIAN_POINT('Ctrl Pts',(6.695691970849,-1.18876479720094,4.906002459825));
#10723=CARTESIAN_POINT('Ctrl Pts',(6.67974554243104,-1.21002352246016,4.90429570169942));
#10724=CARTESIAN_POINT('Ctrl Pts',(6.66979015629161,-1.22296142574569,4.90324105094155));
#10725=CARTESIAN_POINT('Ctrl Pts',(6.58483031207992,-1.33061398973457,4.8943285919645));
#10726=CARTESIAN_POINT('Ctrl Pts',(6.50153550920894,-1.41843997195227,4.8861322351878));
#10727=CARTESIAN_POINT('Ctrl Pts',(6.30126932224092,-1.59448675528496,4.86764966304606));
#10728=CARTESIAN_POINT('Ctrl Pts',(6.18147907553477,-1.67848784591336,4.85733007374101));
#10729=CARTESIAN_POINT('Ctrl Pts',(6.04133884055726,-1.75540441676685,4.84667745020489));
#10730=CARTESIAN_POINT('Ctrl Pts',(6.02901085423549,-1.76200298910028,4.84575184107523));
#10731=CARTESIAN_POINT('Ctrl Pts',(6.00712143869961,-1.7734248675481,4.84412982981531));
#10732=CARTESIAN_POINT('Ctrl Pts',(5.9975887663511,-1.77830176613695,4.84343055316382));
#10733=CARTESIAN_POINT('Ctrl Pts',(5.98311076227342,-1.78556219556864,4.84237971579656));
#10734=CARTESIAN_POINT('Ctrl Pts',(5.97819428164566,-1.78800237009174,4.84202480854908));
#10735=CARTESIAN_POINT('Ctrl Pts',(5.97325426947437,-1.79042886310762,4.84167018981195));
#10736=CARTESIAN_POINT('Ctrl Pts',(5.97324081758061,-1.79043547037812,4.8416692241826));
#10737=CARTESIAN_POINT('Ctrl Pts',(5.97321461181638,-1.79044834169904,4.84166734305946));
#10738=CARTESIAN_POINT('Ctrl Pts',(5.97320185797123,-1.79045460575605,4.841666427566));
#10739=CARTESIAN_POINT('Ctrl Pts',(5.97317618545032,-1.79046721448624,4.84166458477392));
#10740=CARTESIAN_POINT('Ctrl Pts',(5.97316326678685,-1.79047355914897,4.84166365747654));
#10741=CARTESIAN_POINT('Ctrl Pts',(5.97313726220864,-1.7904863302662,4.8416617909039));
#10742=CARTESIAN_POINT('Ctrl Pts',(5.97312417631221,-1.79049275670717,4.84166085163032));
#10743=CARTESIAN_POINT('Ctrl Pts',(5.97309783483001,-1.79050569256458,4.84165896093136));
#10744=CARTESIAN_POINT('Ctrl Pts',(5.97308457922809,-1.7905122019843,4.84165800950519));
#10745=CARTESIAN_POINT('Ctrl Pts',(5.97305789585658,-1.79052530500224,4.84165609432428));
#10746=CARTESIAN_POINT('Ctrl Pts',(5.97304446805399,-1.79053189861188,4.84165513056754));
#10747=CARTESIAN_POINT('Ctrl Pts',(5.97301743774316,-1.79054517124153,4.84165319054445));
#10748=CARTESIAN_POINT('Ctrl Pts',(5.97300383520166,-1.79055185027297,4.8416522142761));
#10749=CARTESIAN_POINT('Ctrl Pts',(5.97297645274663,-1.79056529504064,4.84165024903959));
#10750=CARTESIAN_POINT('Ctrl Pts',(5.97296267291844,-1.79057206072993,4.84164926007794));
#10751=CARTESIAN_POINT('Ctrl Pts',(5.97293493329572,-1.79058568007188,4.84164726926984));
#10752=CARTESIAN_POINT('Ctrl Pts',(5.97292097347083,-1.79059253373426,4.84164626742161));
#10753=CARTESIAN_POINT('Ctrl Pts',(5.97289287121183,-1.7906063303043,4.84164425065191));
#10754=CARTESIAN_POINT('Ctrl Pts',(5.97287872875385,-1.79061327321834,4.84164323572913));
#10755=CARTESIAN_POINT('Ctrl Pts',(5.97285025849024,-1.79062724962001,4.84164119261506));
#10756=CARTESIAN_POINT('Ctrl Pts',(5.97283593068016,-1.79063428310434,4.84164016442388));
#10757=CARTESIAN_POINT('Ctrl Pts',(5.97280708694354,-1.79064844198926,4.84163809457561));
#10758=CARTESIAN_POINT('Ctrl Pts',(5.97279257100046,-1.79065556739233,4.84163705291778));
#10759=CARTESIAN_POINT('Ctrl Pts',(5.97276334814837,-1.79066991149647,4.84163495593306));
#10760=CARTESIAN_POINT('Ctrl Pts',(5.97274864127561,-1.79067713017394,4.84163390060922));
#10761=CARTESIAN_POINT('Ctrl Pts',(5.972719033695,-1.79069166221769,4.84163177608799));
#10762=CARTESIAN_POINT('Ctrl Pts',(5.97270413299984,-1.79069897557178,4.84163070689197));
#10763=CARTESIAN_POINT('Ctrl Pts',(5.97267413494835,-1.79071369833788,4.841628554425));
#10764=CARTESIAN_POINT('Ctrl Pts',(5.97265903748002,-1.79072110779872,4.84162747114649));
#10765=CARTESIAN_POINT('Ctrl Pts',(5.97262864285379,-1.7907360242461,4.84162529029869));
#10766=CARTESIAN_POINT('Ctrl Pts',(5.97261334573714,-1.79074353120609,4.84162419273285));
#10767=CARTESIAN_POINT('Ctrl Pts',(5.97258254877119,-1.79075864412614,4.84162198309354));
#10768=CARTESIAN_POINT('Ctrl Pts',(5.97256704892172,-1.7907662500798,4.84162087102057));
#10769=CARTESIAN_POINT('Ctrl Pts',(5.97253584340905,-1.79078156247958,4.84161863214748));
#10770=CARTESIAN_POINT('Ctrl Pts',(5.97252013777952,-1.7907892689025,4.8416175053503));
#10771=CARTESIAN_POINT('Ctrl Pts',(5.97248851759955,-1.79080478374535,4.84161523680743));
#10772=CARTESIAN_POINT('Ctrl Pts',(5.97247260303742,-1.79081259216413,4.84161409506145));
#10773=CARTESIAN_POINT('Ctrl Pts',(5.97244056176071,-1.79082831256356,4.84161179639079));
#10774=CARTESIAN_POINT('Ctrl Pts',(5.97242443513319,-1.79083622449442,4.8416106394729));
#10775=CARTESIAN_POINT('Ctrl Pts',(5.97239196658779,-1.79085215343624,4.84160831023497));
#10776=CARTESIAN_POINT('Ctrl Pts',(5.97237562455932,-1.79086017049419,4.84160713790757));
#10777=CARTESIAN_POINT('Ctrl Pts',(5.97234272188251,-1.79087631130167,4.84160477761348));
#10778=CARTESIAN_POINT('Ctrl Pts',(5.97232616127637,-1.79088443502304,4.84160358965042));
#10779=CARTESIAN_POINT('Ctrl Pts',(5.97229281805885,-1.79090079079554,4.84160119784393));
#10780=CARTESIAN_POINT('Ctrl Pts',(5.9722760354639,-1.79090902283092,4.84159999400228));
#10781=CARTESIAN_POINT('Ctrl Pts',(5.97224224488607,-1.79092559686754,4.84159757019782));
#10782=CARTESIAN_POINT('Ctrl Pts',(5.97222523689052,-1.79093393886708,4.84159635023471));
#10783=CARTESIAN_POINT('Ctrl Pts',(5.97219099203734,-1.79095073451215,4.84159389393999));
#10784=CARTESIAN_POINT('Ctrl Pts',(5.97217375518661,-1.79095918814617,4.84159265760952));
#10785=CARTESIAN_POINT('Ctrl Pts',(5.97213904914235,-1.79097620874276,4.84159016833233));
#10786=CARTESIAN_POINT('Ctrl Pts',(5.9721215798687,-1.79098477573626,4.84158891538053));
#10787=CARTESIAN_POINT('Ctrl Pts',(5.97208640533138,-1.79100202481519,4.8415863926011));
#10788=CARTESIAN_POINT('Ctrl Pts',(5.97206870011,-1.79101070687127,4.84158512277717));
#10789=CARTESIAN_POINT('Ctrl Pts',(5.97203305003128,-1.79102818783726,4.84158256599404));
#10790=CARTESIAN_POINT('Ctrl Pts',(5.97201510513642,-1.79103698675669,4.84158127903284));
#10791=CARTESIAN_POINT('Ctrl Pts',(5.97197897197081,-1.79105470325643,4.84157868770903));
#10792=CARTESIAN_POINT('Ctrl Pts',(5.97196078372762,-1.79106362081412,4.84157738334913));
#10793=CARTESIAN_POINT('Ctrl Pts',(5.97192416011175,-1.79108157640323,4.8415747569609));
#10794=CARTESIAN_POINT('Ctrl Pts',(5.97190572468066,-1.7910906144539,4.84157343492912));
#10795=CARTESIAN_POINT('Ctrl Pts',(5.97186860280112,-1.79110881290672,4.84157077292057));
#10796=CARTESIAN_POINT('Ctrl Pts',(5.97184991638432,-1.79111797328368,4.84156943294682));
#10797=CARTESIAN_POINT('Ctrl Pts',(5.96779173482544,-1.79310727927813,4.84127843327595));
#10798=CARTESIAN_POINT('Ctrl Pts',(5.96374560892815,-1.79507372718939,4.84098963761113));
#10799=CARTESIAN_POINT('Ctrl Pts',(5.95458621933872,-1.79948701771378,4.84033887643599));
#10800=CARTESIAN_POINT('Ctrl Pts',(5.94946916404042,-1.80192576096321,4.83997740977135));
#10801=CARTESIAN_POINT('Ctrl Pts',(5.93622638961938,-1.80816801881361,4.83904716244677));
#10802=CARTESIAN_POINT('Ctrl Pts',(5.9280851787687,-1.81193863350361,4.83848032727813));
#10803=CARTESIAN_POINT('Ctrl Pts',(5.87556718820647,-1.83583341608546,4.83485436532135));
#10804=CARTESIAN_POINT('Ctrl Pts',(5.83048717443688,-1.85438256021371,4.83188184274893));
#10805=CARTESIAN_POINT('Ctrl Pts',(5.77122186882622,-1.87626557697511,4.8280968443184));
#10806=CARTESIAN_POINT('Ctrl Pts',(5.75762042331226,-1.88112057705133,4.82723640218582));
#10807=CARTESIAN_POINT('Ctrl Pts',(5.63162341461277,-1.92455811420703,4.81933128304467));
#10808=CARTESIAN_POINT('Ctrl Pts',(5.51603999125919,-1.95317367974293,4.81254496577493));
#10809=CARTESIAN_POINT('Ctrl Pts',(5.30724346848137,-1.98545339295984,4.80017396451355));
#10810=CARTESIAN_POINT('Ctrl Pts',(5.21503321011211,-1.99320793024042,4.79467512054944));
#10811=CARTESIAN_POINT('Ctrl Pts',(5.09975311288965,-1.99487233749274,4.78756487535699));
#10812=CARTESIAN_POINT('Ctrl Pts',(5.0768787692345,-1.99480912505917,4.7861429138952));
#10813=CARTESIAN_POINT('Ctrl Pts',(5.04341392610554,-1.99414102243853,4.7840441928695));
#10814=CARTESIAN_POINT('Ctrl Pts',(5.03281859943143,-1.99384499403104,4.78337701766936));
#10815=CARTESIAN_POINT('Ctrl Pts',(5.01412969635665,-1.99317372976244,4.78219522791565));
#10816=CARTESIAN_POINT('Ctrl Pts',(5.00603504223436,-1.99283359659311,4.78168171726847));
#10817=CARTESIAN_POINT('Ctrl Pts',(4.98913692104654,-1.99202039147902,4.78060619342338));
#10818=CARTESIAN_POINT('Ctrl Pts',(4.98033408592948,-1.99153825078043,4.78004390837229));
#10819=CARTESIAN_POINT('Ctrl Pts',(4.95735472159103,-1.99012679796126,4.77857071282173));
#10820=CARTESIAN_POINT('Ctrl Pts',(4.94318461503148,-1.98910437255734,4.77765692097764));
#10821=CARTESIAN_POINT('Ctrl Pts',(4.88429038086476,-1.98422201786818,4.77383597582742));
#10822=CARTESIAN_POINT('Ctrl Pts',(4.83969500769983,-1.97900454641532,4.77088701057705));
#10823=CARTESIAN_POINT('Ctrl Pts',(4.60755187933135,-1.94386908882395,4.75523365450591));
#10824=CARTESIAN_POINT('Ctrl Pts',(4.42481948914022,-1.88878180565106,4.74174447563576));
#10825=CARTESIAN_POINT('Ctrl Pts',(4.20295810335114,-1.78560546430026,4.72496613757666));
#10826=CARTESIAN_POINT('Ctrl Pts',(4.15420544056685,-1.76043936465509,4.7212617997646));
#10827=CARTESIAN_POINT('Ctrl Pts',(4.09805239799195,-1.72845473708438,4.71702453683944));
#10828=CARTESIAN_POINT('Ctrl Pts',(4.08959265983707,-1.72355337396047,4.71638699834109));
#10829=CARTESIAN_POINT('Ctrl Pts',(4.07659057567029,-1.71589205500446,4.7154088254445));
#10830=CARTESIAN_POINT('Ctrl Pts',(4.07202278983582,-1.71317589396691,4.71506550544436));
#10831=CARTESIAN_POINT('Ctrl Pts',(4.06360577520608,-1.70812521069914,4.71443355061349));
#10832=CARTESIAN_POINT('Ctrl Pts',(4.05975361115117,-1.70579592372634,4.71414460017078));
#10833=CARTESIAN_POINT('Ctrl Pts',(4.05102688093056,-1.70047870819988,4.7134906001621));
#10834=CARTESIAN_POINT('Ctrl Pts',(4.04615725891464,-1.6974828539401,4.71312607157251));
#10835=CARTESIAN_POINT('Ctrl Pts',(4.03354203295897,-1.68964683896085,4.71218261373066));
#10836=CARTESIAN_POINT('Ctrl Pts',(4.02581657081383,-1.68477428159878,4.71160572315657));
#10837=CARTESIAN_POINT('Ctrl Pts',(3.97429964627373,-1.65178507098262,4.70776271936707));
#10838=CARTESIAN_POINT('Ctrl Pts',(3.93158538720874,-1.62201444338199,4.70459551910765));
#10839=CARTESIAN_POINT('Ctrl Pts',(3.84716859039364,-1.55812903618492,4.69826996929578));
#10840=CARTESIAN_POINT('Ctrl Pts',(3.80558608938803,-1.52392885665618,4.69511807250601));
#10841=CARTESIAN_POINT('Ctrl Pts',(3.6914377605992,-1.42203051817702,4.68620774371435));
#10842=CARTESIAN_POINT('Ctrl Pts',(3.6224719221804,-1.35054804798122,4.68049863373865));
#10843=CARTESIAN_POINT('Ctrl Pts',(3.52541315284806,-1.23364812816854,4.67151574501245));
#10844=CARTESIAN_POINT('Ctrl Pts',(3.49334164844884,-1.19174482408826,4.66835854377184));
#10845=CARTESIAN_POINT('Ctrl Pts',(3.44305203555003,-1.1203417164278,4.66303285188453));
#10846=CARTESIAN_POINT('Ctrl Pts',(3.42387407191304,-1.09154960281792,4.66089921627786));
#10847=CARTESIAN_POINT('Ctrl Pts',(3.39881922910334,-1.05172761184657,4.65795906685079));
#10848=CARTESIAN_POINT('Ctrl Pts',(3.39228238712628,-1.04111873967821,4.65717682544423));
#10849=CARTESIAN_POINT('Ctrl Pts',(3.38148521452398,-1.02322230441606,4.65585862376941));
#10850=CARTESIAN_POINT('Ctrl Pts',(3.37717091296617,-1.01596759225094,4.65532463938377));
#10851=CARTESIAN_POINT('Ctrl Pts',(3.36875849814875,-1.00161512576402,4.65426885629764));
#10852=CARTESIAN_POINT('Ctrl Pts',(3.36465782584373,-0.994519059057538,
4.65374716349192));
#10853=CARTESIAN_POINT('Ctrl Pts',(3.35573528511954,-0.978856904206022,
4.652596267491));
#10854=CARTESIAN_POINT('Ctrl Pts',(3.35093279482576,-0.970280078440811,
4.65196638692575));
#10855=CARTESIAN_POINT('Ctrl Pts',(3.33430996787674,-0.940071527132777,
4.64974893019714));
#10856=CARTESIAN_POINT('Ctrl Pts',(3.32282778476937,-0.918257234436943,
4.64814950040768));
#10857=CARTESIAN_POINT('Ctrl Pts',(3.244279143585,-0.762071361410633,4.63670607687237));
#10858=CARTESIAN_POINT('Ctrl Pts',(3.19218384871628,-0.620739336039943,
4.62633888902752));
#10859=CARTESIAN_POINT('Ctrl Pts',(3.13621271217059,-0.392417245021813,
4.60994954107252));
#10860=CARTESIAN_POINT('Ctrl Pts',(3.12127590716206,-0.30868878652656,4.6040235406184));
#10861=CARTESIAN_POINT('Ctrl Pts',(3.1088239824134,-0.198632994791531,4.59651213476653));
#10862=CARTESIAN_POINT('Ctrl Pts',(3.10642169745108,-0.172951839554206,
4.59477921863489));
#10863=CARTESIAN_POINT('Ctrl Pts',(3.10324022679456,-0.129965196569153,
4.59191916817871));
#10864=CARTESIAN_POINT('Ctrl Pts',(3.10218719938283,-0.112683658375299,
4.59078030468028));
#10865=CARTESIAN_POINT('Ctrl Pts',(3.10103960740373,-0.0887131984822156,
4.5892177649745));
#10866=CARTESIAN_POINT('Ctrl Pts',(3.10075351456413,-0.082034799494594,
4.58878426757865));
#10867=CARTESIAN_POINT('Ctrl Pts',(3.10032562681002,-0.0707161060020321,
4.58805282830292));
#10868=CARTESIAN_POINT('Ctrl Pts',(3.10016645157353,-0.0660765598743967,
4.58775393910452));
#10869=CARTESIAN_POINT('Ctrl Pts',(3.09989230295485,-0.0571795792539851,
4.5871826085624));
#10870=CARTESIAN_POINT('Ctrl Pts',(3.09977476597956,-0.0529222935228022,
4.5869100210713));
#10871=CARTESIAN_POINT('Ctrl Pts',(3.09952602345727,-0.0427294365643947,
4.58625923195428));
#10872=CARTESIAN_POINT('Ctrl Pts',(3.09940767935907,-0.0367935503396157,
4.58588173664157));
#10873=CARTESIAN_POINT('Ctrl Pts',(3.09907660892048,-0.0153941640765726,
4.58452594373036));
#10874=CARTESIAN_POINT('Ctrl Pts',(3.09901720150257,7.16218653557497E-5,
4.58355570142605));
#10875=CARTESIAN_POINT('Ctrl Pts',(3.10016409170935,0.147312245682319,4.57439692124935));
#10876=CARTESIAN_POINT('Ctrl Pts',(3.11424635515854,0.278680929092709,4.56680859138581));
#10877=CARTESIAN_POINT('Ctrl Pts',(3.16964955494612,0.54401935990359,4.55107124596365));
#10878=CARTESIAN_POINT('Ctrl Pts',(3.21229905976571,0.676950336641671,4.54294362226343));
#10879=CARTESIAN_POINT('Ctrl Pts',(3.27627359279887,0.822133984055138,4.53312161123617));
#10880=CARTESIAN_POINT('Ctrl Pts',(3.28436926009618,0.839801955480722,4.53191018164853));
#10881=CARTESIAN_POINT('Ctrl Pts',(3.29699056000783,0.866316608245543,4.53006629907485));
#10882=CARTESIAN_POINT('Ctrl Pts',(3.30132641995931,0.875252720065993,4.52944036382479));
#10883=CARTESIAN_POINT('Ctrl Pts',(3.30928746784373,0.891352975719818,4.52830427127814));
#10884=CARTESIAN_POINT('Ctrl Pts',(3.3128895369032,0.89852836334888,4.5277949251043));
#10885=CARTESIAN_POINT('Ctrl Pts',(3.32071323456913,0.913881436945375,4.5266984772613));
#10886=CARTESIAN_POINT('Ctrl Pts',(3.32494832199605,0.922052018655944,4.52611091332138));
#10887=CARTESIAN_POINT('Ctrl Pts',(3.33649777280483,0.94396146965767,4.52452424259157));
#10888=CARTESIAN_POINT('Ctrl Pts',(3.34391652981032,0.957644294547188,4.52352147819668));
#10889=CARTESIAN_POINT('Ctrl Pts',(3.38106899637459,1.02429316675204,4.51857743566589));
#10890=CARTESIAN_POINT('Ctrl Pts',(3.4130484331492,1.07596403141138,4.51455670711693));
#10891=CARTESIAN_POINT('Ctrl Pts',(3.46230162440845,1.14797871692089,4.50867389836942));
#10892=CARTESIAN_POINT('Ctrl Pts',(3.47770542095237,1.16956451007768,4.50687264275241));
#10893=CARTESIAN_POINT('Ctrl Pts',(3.58242573665211,1.31029180932618,4.49488144139735));
#10894=CARTESIAN_POINT('Ctrl Pts',(3.68440405461566,1.41940861574163,4.48433660699607));
#10895=CARTESIAN_POINT('Ctrl Pts',(3.83609668502084,1.54910012507296,4.47068521047233));
#10896=CARTESIAN_POINT('Ctrl Pts',(3.87587101771571,1.58056348912742,4.46726923857692));
#10897=CARTESIAN_POINT('Ctrl Pts',(3.92454392406315,1.6161361888765,4.463317799071));
#10898=CARTESIAN_POINT('Ctrl Pts',(3.93232422734655,1.62173685073044,4.46269286259712));
#10899=CARTESIAN_POINT('Ctrl Pts',(3.94444664968546,1.63033120044091,4.46172986215833));
#10900=CARTESIAN_POINT('Ctrl Pts',(3.9487606488812,1.6333640339037,4.46138923923341));
#10901=CARTESIAN_POINT('Ctrl Pts',(3.95678296653972,1.63895649026087,4.46075973892991));
#10902=CARTESIAN_POINT('Ctrl Pts',(3.96048790790836,1.64152064108349,4.46047056590162));
#10903=CARTESIAN_POINT('Ctrl Pts',(3.96895923789559,1.64734120667784,4.45981286443535));
#10904=CARTESIAN_POINT('Ctrl Pts',(3.97373109129877,1.65058949840283,4.45944488185673));
#10905=CARTESIAN_POINT('Ctrl Pts',(3.98624151273063,1.65902634406777,4.45848645674469));
#10906=CARTESIAN_POINT('Ctrl Pts',(3.99400255271682,1.66418154579543,4.45789816089755));
#10907=CARTESIAN_POINT('Ctrl Pts',(4.04861538771135,1.69990870869614,4.45380008672563));
#10908=CARTESIAN_POINT('Ctrl Pts',(4.09670361270046,1.72855521529318,4.45040472929386));
#10909=CARTESIAN_POINT('Ctrl Pts',(4.28899021322516,1.83240224929677,4.43738613443141));
#10910=CARTESIAN_POINT('Ctrl Pts',(4.44095393201731,1.89188330190286,4.42822645789346));
#10911=CARTESIAN_POINT('Ctrl Pts',(4.66372079266504,1.9489933577245,4.4145353423935));
#10912=CARTESIAN_POINT('Ctrl Pts',(4.72978223251753,1.96240578313709,4.41045210959053));
#10913=CARTESIAN_POINT('Ctrl Pts',(4.81180618877112,1.97477461289938,4.40529206079465));
#10914=CARTESIAN_POINT('Ctrl Pts',(4.82724784978449,1.9769183214168,4.40431686097244));
#10915=CARTESIAN_POINT('Ctrl Pts',(4.85175956841584,1.98002879002063,4.40276220237625));
#10916=CARTESIAN_POINT('Ctrl Pts',(4.86081406428668,1.98111474198218,4.40218648772142));
#10917=CARTESIAN_POINT('Ctrl Pts',(4.87786308993262,1.98304102323914,4.4010996263888));
#10918=CARTESIAN_POINT('Ctrl Pts',(4.8858558960803,1.98389519119144,4.4005889246598));
#10919=CARTESIAN_POINT('Ctrl Pts',(4.90385542346344,1.98570877939338,4.39943611933404));
#10920=CARTESIAN_POINT('Ctrl Pts',(4.91386461538426,1.98664090705762,4.39879317526066));
#10921=CARTESIAN_POINT('Ctrl Pts',(4.93949288858385,1.98883232889451,4.3971419121087));
#10922=CARTESIAN_POINT('Ctrl Pts',(4.95512030760072,1.98998328776442,4.39613024740096));
#10923=CARTESIAN_POINT('Ctrl Pts',(5.05986684368127,1.9964580516727,4.38931600518865));
#10924=CARTESIAN_POINT('Ctrl Pts',(5.14923105906543,1.99597708802232,4.38333417607024));
#10925=CARTESIAN_POINT('Ctrl Pts',(5.368495650465,1.98005996633097,4.36827257613832));
#10926=CARTESIAN_POINT('Ctrl Pts',(5.49748587795039,1.95783981502472,4.35906244333095));
#10927=CARTESIAN_POINT('Ctrl Pts',(5.68424958192619,1.90641434137607,4.34572060510302));
#10928=CARTESIAN_POINT('Ctrl Pts',(5.74430112269613,1.88676961786906,4.34143511563473));
#10929=CARTESIAN_POINT('Ctrl Pts',(5.8127627901207,1.86071520788417,4.33662915270703));
#10930=CARTESIAN_POINT('Ctrl Pts',(5.8221732581293,1.85705182927412,4.33597035543761));
#10931=CARTESIAN_POINT('Ctrl Pts',(5.83655672865267,1.85132636679246,4.33496663904351));
#10932=CARTESIAN_POINT('Ctrl Pts',(5.84154971656284,1.84931541618558,4.33461881478507));
#10933=CARTESIAN_POINT('Ctrl Pts',(5.85069908495199,1.8455873502659,4.33398262957089));
#10934=CARTESIAN_POINT('Ctrl Pts',(5.85485779268381,1.84387639366469,4.33369392004714));
#10935=CARTESIAN_POINT('Ctrl Pts',(5.86421235044143,1.83999074399096,4.33304551340429));
#10936=CARTESIAN_POINT('Ctrl Pts',(5.86940478951236,1.83780810261645,4.33268629879851));
#10937=CARTESIAN_POINT('Ctrl Pts',(5.88466537433436,1.83131712176445,4.33163242379357));
#10938=CARTESIAN_POINT('Ctrl Pts',(5.89470755775693,1.82694775044492,4.33094131300108));
#10939=CARTESIAN_POINT('Ctrl Pts',(5.99276781497663,1.78331762217945,4.32421137891598));
#10940=CARTESIAN_POINT('Ctrl Pts',(6.0778796060278,1.73780374911271,4.31851501711611));
#10941=CARTESIAN_POINT('Ctrl Pts',(6.26786680947022,1.61775408209795,4.30540006562914));
#10942=CARTESIAN_POINT('Ctrl Pts',(6.3694839418109,1.53889442004371,4.29805211889814));
#10943=CARTESIAN_POINT('Ctrl Pts',(6.50701258713228,1.40912248299074,4.28674784902604));
#10944=CARTESIAN_POINT('Ctrl Pts',(6.54927192677593,1.36542984922908,4.28305312174268));
#10945=CARTESIAN_POINT('Ctrl Pts',(6.59947560623293,1.3085407960717,4.27833036670315));
#10946=CARTESIAN_POINT('Ctrl Pts',(6.60935274923855,1.29708844228768,4.27738389452483));
#10947=CARTESIAN_POINT('Ctrl Pts',(6.6249097096193,1.27863015977595,4.27586455379365));
#10948=CARTESIAN_POINT('Ctrl Pts',(6.63067401160961,1.2716959579936,4.27529513878569));
#10949=CARTESIAN_POINT('Ctrl Pts',(6.64149753644228,1.25849466544202,4.27421350687661));
#10950=CARTESIAN_POINT('Ctrl Pts',(6.64656621722854,1.25223553458073,4.27370168560467));
#10951=CARTESIAN_POINT('Ctrl Pts',(6.65797719345753,1.23796872608678,4.27253724849171));
#10952=CARTESIAN_POINT('Ctrl Pts',(6.6642961233049,1.22994273150356,4.27188372129819));
#10953=CARTESIAN_POINT('Ctrl Pts',(6.68048009717417,1.20905858014824,4.27018697265338));
#10954=CARTESIAN_POINT('Ctrl Pts',(6.69025042765089,1.19612830334546,4.26914008583931));
#10955=CARTESIAN_POINT('Ctrl Pts',(6.77707965361206,1.07825743432101,4.2596273351404));
#10956=CARTESIAN_POINT('Ctrl Pts',(6.84383540839038,0.966145834093963,4.25076415439392));
#10957=CARTESIAN_POINT('Ctrl Pts',(6.93881075892006,0.76403090248282,4.23525055538052));
#10958=CARTESIAN_POINT('Ctrl Pts',(6.97247822476205,0.677036417394026,4.22871437547163));
#10959=CARTESIAN_POINT('Ctrl Pts',(7.01730261076583,0.531731169832178,4.21826368859593));
#10960=CARTESIAN_POINT('Ctrl Pts',(7.032163857205,0.474708450966558,4.21427604815709));
#10961=CARTESIAN_POINT('Ctrl Pts',(7.04655994959518,0.407383183415082,4.20976039466402));
#10962=CARTESIAN_POINT('Ctrl Pts',(7.04856635222556,0.397644446517391,4.20911186019882));
#10963=CARTESIAN_POINT('Ctrl Pts',(7.05154018650171,0.382643267487679,4.20812046686881));
#10964=CARTESIAN_POINT('Ctrl Pts',(7.05255937280284,0.377391420711163,4.20777480977541));
#10965=CARTESIAN_POINT('Ctrl Pts',(7.05439674144263,0.367715516887429,4.20714067928));
#10966=CARTESIAN_POINT('Ctrl Pts',(7.05522108354875,0.363292805373047,4.20685187311068));
#10967=CARTESIAN_POINT('Ctrl Pts',(7.0570509391888,0.353287575524319,4.20620086187582));
#10968=CARTESIAN_POINT('Ctrl Pts',(7.0580476078255,0.347703541010868,4.20583915737786));
#10969=CARTESIAN_POINT('Ctrl Pts',(7.06056132499627,0.333264137421996,4.20490788582372));
#10970=CARTESIAN_POINT('Ctrl Pts',(7.06204241027792,0.32440252266112,4.20434027141216));
#10971=CARTESIAN_POINT('Ctrl Pts',(7.07121065976443,0.267171639492199,4.20069793192226));
#10972=CARTESIAN_POINT('Ctrl Pts',(7.07717478663549,0.218538890282222,4.19771071067118));
#10973=CARTESIAN_POINT('Ctrl Pts',(7.0824969622721,0.156217563139525,4.19396412132613));
#10974=CARTESIAN_POINT('Ctrl Pts',(7.08351321349206,0.142691731819713,4.19315586760225));
#10975=CARTESIAN_POINT('Ctrl Pts',(7.0871436593937,0.0867391208870799,4.18982881601366));
#10976=CARTESIAN_POINT('Ctrl Pts',(7.08853944685373,0.0442433067737386,
4.18734086199011));
#10977=CARTESIAN_POINT('Ctrl Pts',(7.08857690420654,0.00115606453166728,
4.18483113989589));
#10978=CARTESIAN_POINT('Ctrl Pts',(7.08857715545314,0.000578028143273556,
4.18479747312931));
#10979=CARTESIAN_POINT('Ctrl Pts',(7.08857715545311,-9.37345802482418E-11,
4.18476380915572));
#10980=CARTESIAN_POINT('Ctrl Pts',(7.08857715492705,4.58116840822842E-5,
4.02544646529617));
#10981=CARTESIAN_POINT('Ctrl Pts',(7.08857709852169,0.00250183564861334,
4.02560187048724));
#10982=CARTESIAN_POINT('Ctrl Pts',(7.08857250616951,0.00495785070224662,
4.02575741631251));
#10983=CARTESIAN_POINT('Ctrl Pts',(7.08854430144895,0.0125464882364174,
4.02623846485478));
#10984=CARTESIAN_POINT('Ctrl Pts',(7.08850541498808,0.0176789997428494,
4.02656444054343));
#10985=CARTESIAN_POINT('Ctrl Pts',(7.0883442039336,0.0317753122926986,4.02746146572168));
#10986=CARTESIAN_POINT('Ctrl Pts',(7.08818126193469,0.0407384437379774,
4.02803377315785));
#10987=CARTESIAN_POINT('Ctrl Pts',(7.08758290353538,0.0647465644321104,
4.02957205024097));
#10988=CARTESIAN_POINT('Ctrl Pts',(7.08703761993958,0.0797879962970355,
4.03054141383691));
#10989=CARTESIAN_POINT('Ctrl Pts',(7.08364312076721,0.151117008065387,4.03516588236312));
#10990=CARTESIAN_POINT('Ctrl Pts',(7.07857969142872,0.20726856435142,4.03888896844737));
#10991=CARTESIAN_POINT('Ctrl Pts',(7.06586609534288,0.302807672359106,4.04536853327583));
#10992=CARTESIAN_POINT('Ctrl Pts',(7.05939255246803,0.342319197734179,4.048090944713));
#10993=CARTESIAN_POINT('Ctrl Pts',(7.03694388477639,0.457496270064081,4.05614236579636));
#10994=CARTESIAN_POINT('Ctrl Pts',(7.01775365014093,0.532457742289129,4.06153308152317));
#10995=CARTESIAN_POINT('Ctrl Pts',(6.97045390472378,0.680763747804374,4.07238436832725));
#10996=CARTESIAN_POINT('Ctrl Pts',(6.94226572929044,0.753951958449263,4.07783549493542));
#10997=CARTESIAN_POINT('Ctrl Pts',(6.89966222109006,0.847698540996847,4.0848089072685));
#10998=CARTESIAN_POINT('Ctrl Pts',(6.88906701568782,0.869912098662336,4.0864603185018));
#10999=CARTESIAN_POINT('Ctrl Pts',(6.87058965905482,0.906874808492847,4.08920001644525));
#11000=CARTESIAN_POINT('Ctrl Pts',(6.86292843116922,0.921730781025356,4.09029887041223));
#11001=CARTESIAN_POINT('Ctrl Pts',(6.85198623558389,0.942309751363044,4.09181604578255));
#11002=CARTESIAN_POINT('Ctrl Pts',(6.84886249949088,0.948114952263243,4.09224347059474));
#11003=CARTESIAN_POINT('Ctrl Pts',(6.8434984938801,0.957966156216981,4.09296769996346));
#11004=CARTESIAN_POINT('Ctrl Pts',(6.84127284285697,0.962020020688211,4.09326540909022));
#11005=CARTESIAN_POINT('Ctrl Pts',(6.8369602364849,0.969810776813559,4.09383688668179));
#11006=CARTESIAN_POINT('Ctrl Pts',(6.83487533728708,0.973548720086075,4.09411078700596));
#11007=CARTESIAN_POINT('Ctrl Pts',(6.82983072216348,0.982525001238606,4.09476790189424));
#11008=CARTESIAN_POINT('Ctrl Pts',(6.82685928442083,0.987756753396547,4.09515037902927));
#11009=CARTESIAN_POINT('Ctrl Pts',(6.81586595085718,1.00691017907661,4.09654902526836));
#11010=CARTESIAN_POINT('Ctrl Pts',(6.80769935346212,1.02074867073847,4.09755643906983));
#11011=CARTESIAN_POINT('Ctrl Pts',(6.73749862823314,1.13648721328408,4.10596864954574));
#11012=CARTESIAN_POINT('Ctrl Pts',(6.66659686688781,1.23274581067569,4.11288624743041));
#11013=CARTESIAN_POINT('Ctrl Pts',(6.51803786695324,1.40058464061019,4.12589836657878));
#11014=CARTESIAN_POINT('Ctrl Pts',(6.4424933612927,1.47346902791223,4.13197178641174));
#11015=CARTESIAN_POINT('Ctrl Pts',(6.31951146787305,1.57470446990719,4.14153503950475));
#11016=CARTESIAN_POINT('Ctrl Pts',(6.27604751175241,1.60759149946494,4.14485895894372));
#11017=CARTESIAN_POINT('Ctrl Pts',(6.21928675888488,1.64699177714022,4.14916284017094));
#11018=CARTESIAN_POINT('Ctrl Pts',(6.20718773365005,1.65519468279194,4.1500781502127));
#11019=CARTESIAN_POINT('Ctrl Pts',(6.18867338735697,1.66745220598004,4.151476147814));
#11020=CARTESIAN_POINT('Ctrl Pts',(6.18232310417629,1.6716045279285,4.1519551845026));
#11021=CARTESIAN_POINT('Ctrl Pts',(6.16935051152475,1.67998177862438,4.15293291787599));
#11022=CARTESIAN_POINT('Ctrl Pts',(6.16272663220396,1.68420401724034,4.15343170263343));
#11023=CARTESIAN_POINT('Ctrl Pts',(6.14813415832408,1.69338489157496,4.15452963383762));
#11024=CARTESIAN_POINT('Ctrl Pts',(6.1401551932842,1.69832661158322,4.15512938675838));
#11025=CARTESIAN_POINT('Ctrl Pts',(6.1177229848562,1.71200176934391,4.15681409422844));
#11026=CARTESIAN_POINT('Ctrl Pts',(6.10319354997353,1.72060808446585,4.15790362410002));
#11027=CARTESIAN_POINT('Ctrl Pts',(6.01532393436398,1.77116047061669,4.16448448015018));
#11028=CARTESIAN_POINT('Ctrl Pts',(5.93949805313887,1.80859147009762,4.17013452134775));
#11029=CARTESIAN_POINT('Ctrl Pts',(5.72398909994932,1.89845526580207,4.18609488797693));
#11030=CARTESIAN_POINT('Ctrl Pts',(5.5804602603567,1.9402113496441,4.19664882535676));
#11031=CARTESIAN_POINT('Ctrl Pts',(5.38366091572784,1.97423281006533,4.21031010996969));
#11032=CARTESIAN_POINT('Ctrl Pts',(5.33337861411253,1.98096311405979,4.21372722070526));
#11033=CARTESIAN_POINT('Ctrl Pts',(5.27334632543013,1.98667872066863,4.21767979426143));
#11034=CARTESIAN_POINT('Ctrl Pts',(5.26379590596213,1.98751857958875,4.21830478364355));
#11035=CARTESIAN_POINT('Ctrl Pts',(5.24898318488842,1.98871364920272,4.21926784786616));
#11036=CARTESIAN_POINT('Ctrl Pts',(5.24372505857129,1.989116887513,4.21960848219264));
#11037=CARTESIAN_POINT('Ctrl Pts',(5.23397142564024,1.98982598432062,4.22023799279811));
#11038=CARTESIAN_POINT('Ctrl Pts',(5.22947650899357,1.99013746204794,4.22052716481127));
#11039=CARTESIAN_POINT('Ctrl Pts',(5.21922075557577,1.99081323219154,4.22118485024384));
#11040=CARTESIAN_POINT('Ctrl Pts',(5.21345937107045,1.9911677516999,4.22155281791148));
#11041=CARTESIAN_POINT('Ctrl Pts',(5.1983955756887,1.99202906528167,4.22251117814042));
#11042=CARTESIAN_POINT('Ctrl Pts',(5.18909088638598,1.99249571665251,4.2230994244898));
#11043=CARTESIAN_POINT('Ctrl Pts',(5.12391072845345,1.99530701041735,4.22719623764638));
#11044=CARTESIAN_POINT('Ctrl Pts',(5.06795608949343,1.99536638452538,4.23059046356859));
#11045=CARTESIAN_POINT('Ctrl Pts',(4.84960444696433,1.98640921900876,4.24360915360744));
#11046=CARTESIAN_POINT('Ctrl Pts',(4.68856265971034,1.95990621663879,4.25276976107664));
#11047=CARTESIAN_POINT('Ctrl Pts',(4.46786451647704,1.89518804706262,4.26646208085342));
#11048=CARTESIAN_POINT('Ctrl Pts',(4.40421999358698,1.87296756328339,4.27054547331167));
#11049=CARTESIAN_POINT('Ctrl Pts',(4.32738638211132,1.84169463918865,4.27570570168349));
#11050=CARTESIAN_POINT('Ctrl Pts',(4.31301660765079,1.83564851479277,4.27668091267777));
#11051=CARTESIAN_POINT('Ctrl Pts',(4.29035582247543,1.82579969981102,4.27823558507285));
#11052=CARTESIAN_POINT('Ctrl Pts',(4.2820172947541,1.82210742613277,4.2788113022401));
#11053=CARTESIAN_POINT('Ctrl Pts',(4.26637696442575,1.81505326609324,4.27989816582913));
#11054=CARTESIAN_POINT('Ctrl Pts',(4.25906957334082,1.81170415725227,4.28040886728339));
#11055=CARTESIAN_POINT('Ctrl Pts',(4.24266980595346,1.80406756546632,4.28156166866341));
#11056=CARTESIAN_POINT('Ctrl Pts',(4.23358924872094,1.79975535895956,4.28220460904056));
#11057=CARTESIAN_POINT('Ctrl Pts',(4.2104385688693,1.78854625255723,4.28385585616723));
#11058=CARTESIAN_POINT('Ctrl Pts',(4.19641662386367,1.78155196586377,4.28486750843468));
#11059=CARTESIAN_POINT('Ctrl Pts',(4.1030685211369,1.73360733542049,4.29168137655293));
#11060=CARTESIAN_POINT('Ctrl Pts',(4.02649686933588,1.68754235487881,4.29766282078443));
#11061=CARTESIAN_POINT('Ctrl Pts',(3.84613728877387,1.56184235729986,4.31272434301702));
#11062=CARTESIAN_POINT('Ctrl Pts',(3.74659855618972,1.47683902506872,4.3219348307558));
#11063=CARTESIAN_POINT('Ctrl Pts',(3.61231539684048,1.33721251239724,4.33527707808051));
#11064=CARTESIAN_POINT('Ctrl Pts',(3.57072766755594,1.289644925758,4.33956262959613));
#11065=CARTESIAN_POINT('Ctrl Pts',(3.52518482629187,1.23227057720689,4.34436865285197));
#11066=CARTESIAN_POINT('Ctrl Pts',(3.51896666226061,1.22431367284508,4.34502745221803));
#11067=CARTESIAN_POINT('Ctrl Pts',(3.50952693977512,1.21204346537878,4.34603117116648));
#11068=CARTESIAN_POINT('Ctrl Pts',(3.50626207738366,1.20776390900997,4.34637899590437));
#11069=CARTESIAN_POINT('Ctrl Pts',(3.50030143034232,1.19988480636251,4.34701518163334));
#11070=CARTESIAN_POINT('Ctrl Pts',(3.49760049863815,1.19628936549466,4.34730389119559));
#11071=CARTESIAN_POINT('Ctrl Pts',(3.49154397581996,1.18816997892694,4.34795229747965));
#11072=CARTESIAN_POINT('Ctrl Pts',(3.48819537754692,1.18364094310834,4.34831151169133));
#11073=CARTESIAN_POINT('Ctrl Pts',(3.47839278168777,1.17026461634209,4.3493653842746));
#11074=CARTESIAN_POINT('Ctrl Pts',(3.4719922824136,1.16137812341069,4.35005649306461));
#11075=CARTESIAN_POINT('Ctrl Pts',(3.4100020041262,1.07379847226471,4.35678455420889));
#11076=CARTESIAN_POINT('Ctrl Pts',(3.36010163269945,0.991217005556853,4.36247925978546));
#11077=CARTESIAN_POINT('Ctrl Pts',(3.25810450965683,0.790965105692136,4.37559396395353));
#11078=CARTESIAN_POINT('Ctrl Pts',(3.21102556893558,0.671238044025972,4.38294317599498));
#11079=CARTESIAN_POINT('Ctrl Pts',(3.15908778847075,0.489390940519344,4.39424914646893));
#11080=CARTESIAN_POINT('Ctrl Pts',(3.14507983140447,0.430235629294735,4.39794420079618));
#11081=CARTESIAN_POINT('Ctrl Pts',(3.13098476502849,0.355676869345259,4.40266732463889));
#11082=CARTESIAN_POINT('Ctrl Pts',(3.12834462031343,0.340785371325787,4.40361382271666));
#11083=CARTESIAN_POINT('Ctrl Pts',(3.12440102863109,0.316969408356208,4.40513319535612));
#11084=CARTESIAN_POINT('Ctrl Pts',(3.1229883021754,0.308063443057399,4.40570261611588));
#11085=CARTESIAN_POINT('Ctrl Pts',(3.12042817308161,0.291185314314506,4.40678425276645));
#11086=CARTESIAN_POINT('Ctrl Pts',(3.11926857190762,0.283215161912105,4.40729607298309));
#11087=CARTESIAN_POINT('Ctrl Pts',(3.11674782939329,0.265121186462534,4.40846049917843));
#11088=CARTESIAN_POINT('Ctrl Pts',(3.11541612997236,0.254993554637581,4.40911401644258));
#11089=CARTESIAN_POINT('Ctrl Pts',(3.11217302480051,0.228773026521777,4.4108107220397));
#11090=CARTESIAN_POINT('Ctrl Pts',(3.11037987447228,0.212666520978772,4.41185757542553));
#11091=CARTESIAN_POINT('Ctrl Pts',(3.09595422304999,0.0669684310689805,
4.42137102453675));
#11092=CARTESIAN_POINT('Ctrl Pts',(3.09584459922837,-0.0635241515526198,
4.43023501217895));
#11093=CARTESIAN_POINT('Ctrl Pts',(3.11746372222519,-0.285833321325941,
4.44575144367755));
#11094=CARTESIAN_POINT('Ctrl Pts',(3.13297384668399,-0.377846324009289,
4.45228967009824));
#11095=CARTESIAN_POINT('Ctrl Pts',(3.16868157619853,-0.525648194615674,
4.46273960996431));
#11096=CARTESIAN_POINT('Ctrl Pts',(3.18502963653073,-0.58222416125124,4.46672467228651));
#11097=CARTESIAN_POINT('Ctrl Pts',(3.20703743763096,-0.647418686649058,
4.47123780265506));
#11098=CARTESIAN_POINT('Ctrl Pts',(3.21028755744028,-0.656814271779177,
4.47188624280263));
#11099=CARTESIAN_POINT('Ctrl Pts',(3.21539440881028,-0.671227677611153,
4.47287752284728));
#11100=CARTESIAN_POINT('Ctrl Pts',(3.21720125436617,-0.676262824528884,
4.47322315999818));
#11101=CARTESIAN_POINT('Ctrl Pts',(3.22056493929564,-0.685519126340224,
4.47385727180544));
#11102=CARTESIAN_POINT('Ctrl Pts',(3.22211579843322,-0.689742270564241,
4.47414607908291));
#11103=CARTESIAN_POINT('Ctrl Pts',(3.22565442465368,-0.699278476875247,
4.47479711521682));
#11104=CARTESIAN_POINT('Ctrl Pts',(3.22765057272135,-0.704588322562702,
4.47515884333502));
#11105=CARTESIAN_POINT('Ctrl Pts',(3.23286711612269,-0.718286873948393,
4.47609021651312));
#11106=CARTESIAN_POINT('Ctrl Pts',(3.23612163073709,-0.726662570803931,
4.47665790821851));
#11107=CARTESIAN_POINT('Ctrl Pts',(3.25748829360405,-0.78056916844642,4.48030187689446));
#11108=CARTESIAN_POINT('Ctrl Pts',(3.27721793429671,-0.825445604307218,
4.48329056028528));
#11109=CARTESIAN_POINT('Ctrl Pts',(3.37229867655185,-1.02174543722544,4.49635519451998));
#11110=CARTESIAN_POINT('Ctrl Pts',(3.46507021711557,-1.16395126086564,4.5058536988342));
#11111=CARTESIAN_POINT('Ctrl Pts',(3.61895413196227,-1.34478421876155,4.51998179647415));
#11112=CARTESIAN_POINT('Ctrl Pts',(3.66586963526371,-1.39450022184614,4.52412043826137));
#11113=CARTESIAN_POINT('Ctrl Pts',(3.72655137947403,-1.45252520774829,4.52934276141503));
#11114=CARTESIAN_POINT('Ctrl Pts',(3.73799005573561,-1.46320820933447,4.53032176382666));
#11115=CARTESIAN_POINT('Ctrl Pts',(3.75630055136633,-1.47990998229503,4.53188109671129));
#11116=CARTESIAN_POINT('Ctrl Pts',(3.76309018918098,-1.48601820125571,4.53245764386057));
#11117=CARTESIAN_POINT('Ctrl Pts',(3.77593285504474,-1.49741335728102,4.53354521908515));
#11118=CARTESIAN_POINT('Ctrl Pts',(3.78197637225338,-1.50271077361714,4.53405579579285));
#11119=CARTESIAN_POINT('Ctrl Pts',(3.79563585994884,-1.5145387323627,4.53520717457566));
#11120=CARTESIAN_POINT('Ctrl Pts',(3.803269374401,-1.52104859201148,4.53584880835404));
#11121=CARTESIAN_POINT('Ctrl Pts',(3.82290009062851,-1.53753550438551,4.53749446394439));
#11122=CARTESIAN_POINT('Ctrl Pts',(3.83496566647921,-1.5474297270172,4.53850179289028));
#11123=CARTESIAN_POINT('Ctrl Pts',(3.91517720073498,-1.61164719073418,4.54517287835131));
#11124=CARTESIAN_POINT('Ctrl Pts',(3.98669532784684,-1.66158894882174,4.5510070727885));
#11125=CARTESIAN_POINT('Ctrl Pts',(4.18662332889657,-1.78254992827892,4.5670002139327));
#11126=CARTESIAN_POINT('Ctrl Pts',(4.31997294583062,-1.84435590972678,4.57737512345643));
#11127=CARTESIAN_POINT('Ctrl Pts',(4.50664294086914,-1.90703446154237,4.59084165991703));
#11128=CARTESIAN_POINT('Ctrl Pts',(4.55499790894734,-1.92125733047917,4.5942360688566));
#11129=CARTESIAN_POINT('Ctrl Pts',(4.61312148182262,-1.93598585232027,4.59816602976758));
#11130=CARTESIAN_POINT('Ctrl Pts',(4.62241619364844,-1.93827007377864,4.59878996123502));
#11131=CARTESIAN_POINT('Ctrl Pts',(4.63685386782449,-1.94170820413684,4.59975175076874));
#11132=CARTESIAN_POINT('Ctrl Pts',(4.64198541939511,-1.94290874276813,4.60009215780698));
#11133=CARTESIAN_POINT('Ctrl Pts',(4.65151344300547,-1.9450980560474,4.60072146446842));
#11134=CARTESIAN_POINT('Ctrl Pts',(4.65590848043457,-1.94609226465297,4.60101065813491));
#11135=CARTESIAN_POINT('Ctrl Pts',(4.66594588263913,-1.94832711635444,4.6016686685364));
#11136=CARTESIAN_POINT('Ctrl Pts',(4.67159028958026,-1.94955814661992,4.60203693735338));
#11137=CARTESIAN_POINT('Ctrl Pts',(4.68636637983322,-1.95271359064234,4.6029966059093));
#11138=CARTESIAN_POINT('Ctrl Pts',(4.69550648184458,-1.95459850087827,4.60358584987261));
#11139=CARTESIAN_POINT('Ctrl Pts',(4.75989625093131,-1.96740680047743,4.60770829874435));
#11140=CARTESIAN_POINT('Ctrl Pts',(4.81557901150069,-1.97605126315098,4.61112553013966));
#11141=CARTESIAN_POINT('Ctrl Pts',(5.03278478737302,-2.00040551285652,4.62414231536013));
#11142=CARTESIAN_POINT('Ctrl Pts',(5.19561717009188,-1.99874771707183,4.63328400376623));
#11143=CARTESIAN_POINT('Ctrl Pts',(5.42319137411066,-1.96852195680953,4.64695184671766));
#11144=CARTESIAN_POINT('Ctrl Pts',(5.48942721489577,-1.95628695511843,4.65103198853302));
#11145=CARTESIAN_POINT('Ctrl Pts',(5.57007731849368,-1.93712577578741,4.65618856291183));
#11146=CARTESIAN_POINT('Ctrl Pts',(5.58519822250771,-1.93334553090129,4.65716354866106));
#11147=CARTESIAN_POINT('Ctrl Pts',(5.6090928017212,-1.92707343553369,4.65871794417281));
#11148=CARTESIAN_POINT('Ctrl Pts',(5.61789655834378,-1.92469789023318,4.65929361201861));
#11149=CARTESIAN_POINT('Ctrl Pts',(5.63442993335875,-1.92011479229683,4.66038043347526));
#11150=CARTESIAN_POINT('Ctrl Pts',(5.64216312040221,-1.91792070887504,4.66089114249958));
#11151=CARTESIAN_POINT('Ctrl Pts',(5.65953788285447,-1.91287741672792,4.66204402917443));
#11152=CARTESIAN_POINT('Ctrl Pts',(5.66917154808532,-1.91000195347986,4.66268704780022));
#11153=CARTESIAN_POINT('Ctrl Pts',(5.69376721135482,-1.90245765933255,4.664338629952));
#11154=CARTESIAN_POINT('Ctrl Pts',(5.70869644416392,-1.8976851558804,4.66535054130215));
#11155=CARTESIAN_POINT('Ctrl Pts',(5.80838276081461,-1.86451811328965,4.67217213248661));
#11156=CARTESIAN_POINT('Ctrl Pts',(5.89119334047811,-1.83063397073732,4.6781615204004));
#11157=CARTESIAN_POINT('Ctrl Pts',(6.08862437713143,-1.73390691508636,4.69322463796165));
#11158=CARTESIAN_POINT('Ctrl Pts',(6.19988012040535,-1.66514216001331,4.70242779208748));
#11159=CARTESIAN_POINT('Ctrl Pts',(6.353809332506,-1.54772639908053,4.71576158880403));
#11160=CARTESIAN_POINT('Ctrl Pts',(6.40215814154306,-1.5070779053753,4.72004585996782));
#11161=CARTESIAN_POINT('Ctrl Pts',(6.45591380912792,-1.45734329089058,4.7248506402328));
#11162=CARTESIAN_POINT('Ctrl Pts',(6.46327357481374,-1.45042960338276,4.72550939810109));
#11163=CARTESIAN_POINT('Ctrl Pts',(6.47447565160237,-1.43974520802031,4.72651306725245));
#11164=CARTESIAN_POINT('Ctrl Pts',(6.47835560007893,-1.43601445731111,4.72686088325526));
#11165=CARTESIAN_POINT('Ctrl Pts',(6.48544936001788,-1.42913800066806,4.727497060634));
#11166=CARTESIAN_POINT('Ctrl Pts',(6.48866763050755,-1.42599713714078,4.72778577051755));
#11167=CARTESIAN_POINT('Ctrl Pts',(6.49589303887598,-1.41889765200411,4.72843418699341));
#11168=CARTESIAN_POINT('Ctrl Pts',(6.49989404226039,-1.41493293127675,4.7287934110044));
#11169=CARTESIAN_POINT('Ctrl Pts',(6.51162481274837,-1.40320964476914,4.72984733933442));
#11170=CARTESIAN_POINT('Ctrl Pts',(6.51930768727117,-1.39540416021821,4.73053849351095));
#11171=CARTESIAN_POINT('Ctrl Pts',(6.58997102679856,-1.32242040595063,4.73690841028084));
#11172=CARTESIAN_POINT('Ctrl Pts',(6.64851345431889,-1.25307503632279,4.74228485360505));
#11173=CARTESIAN_POINT('Ctrl Pts',(6.77105869299919,-1.0860455927663,4.7543970671153));
#11174=CARTESIAN_POINT('Ctrl Pts',(6.83161239416044,-0.986257041083104,
4.76106907678195));
#11175=CARTESIAN_POINT('Ctrl Pts',(6.9054470777902,-0.8364293587969,4.77096155112508));
#11176=CARTESIAN_POINT('Ctrl Pts',(6.92605149798289,-0.790274782157797,
4.77399093000325));
#11177=CARTESIAN_POINT('Ctrl Pts',(6.95737387210527,-0.712281559085304,
4.77912099787863));
#11178=CARTESIAN_POINT('Ctrl Pts',(6.96908037166673,-0.68086456606297,4.78119016695826));
#11179=CARTESIAN_POINT('Ctrl Pts',(6.98399671085792,-0.637525098993796,
4.78405516217971));
#11180=CARTESIAN_POINT('Ctrl Pts',(6.98789622250901,-0.625844675980574,
4.78482832777026));
#11181=CARTESIAN_POINT('Ctrl Pts',(6.99427659863734,-0.60612722350328,4.78613553283714));
#11182=CARTESIAN_POINT('Ctrl Pts',(6.99681526280512,-0.598109151358696,
4.78666766950205));
#11183=CARTESIAN_POINT('Ctrl Pts',(7.00173461289452,-0.582223547725681,
4.78772317160442));
#11184=CARTESIAN_POINT('Ctrl Pts',(7.00411752621209,-0.574356876654398,
4.78824645227647));
#11185=CARTESIAN_POINT('Ctrl Pts',(7.00979504188972,-0.555187556437833,
4.78952310627933));
#11186=CARTESIAN_POINT('Ctrl Pts',(7.01303830126534,-0.543870143198756,
4.7902781267716));
#11187=CARTESIAN_POINT('Ctrl Pts',(7.02196835550385,-0.511633667668831,
4.79243270153997));
#11188=CARTESIAN_POINT('Ctrl Pts',(7.02741444346134,-0.490650217271119,
4.79383991517465));
#11189=CARTESIAN_POINT('Ctrl Pts',(7.0697655595526,-0.315802065917204,4.80560876877572));
#11190=CARTESIAN_POINT('Ctrl Pts',(7.08857715545348,-0.158164795785966,
4.81656162480003));
#11191=CARTESIAN_POINT('Ctrl Pts',(7.08857715545311,4.63462601629772E-12,
4.82758772788682));
#11192=CARTESIAN_POINT('Origin',(5.09382715545311,0.,-6.77268258743872));
#11193=CARTESIAN_POINT('',(7.08857697542999,-0.000847468688046533,5.78712926957393));
#11194=CARTESIAN_POINT('',(7.09089102510648,-0.00118553947171295,5.62731851852589));
#11195=CARTESIAN_POINT('',(7.08857715545311,8.3550772080578E-14,-6.77268258743872));
#11196=CARTESIAN_POINT('Ctrl Pts',(7.08857697543024,-0.000847467537915952,
5.78712926964943));
#11197=CARTESIAN_POINT('Ctrl Pts',(7.08851864778083,-0.138137762372735,
5.77811573517358));
#11198=CARTESIAN_POINT('Ctrl Pts',(7.07428701488024,-0.275032252711523,
5.7686626804473));
#11199=CARTESIAN_POINT('Ctrl Pts',(7.02136446103858,-0.527429070389755,
5.7506905530694));
#11200=CARTESIAN_POINT('Ctrl Pts',(6.98594481453895,-0.643022093466309,
5.74224390314858));
#11201=CARTESIAN_POINT('Ctrl Pts',(6.93423458573705,-0.769535208304726,
5.73318740374307));
#11202=CARTESIAN_POINT('Ctrl Pts',(6.92799797685692,-0.784283993764439,
5.73213491133118));
#11203=CARTESIAN_POINT('Ctrl Pts',(6.91917735469631,-0.804462754298365,
5.73070105471366));
#11204=CARTESIAN_POINT('Ctrl Pts',(6.91674558735057,-0.809958064234257,
5.73031120142937));
#11205=CARTESIAN_POINT('Ctrl Pts',(6.91254014790502,-0.819346639230769,
5.72964633515278));
#11206=CARTESIAN_POINT('Ctrl Pts',(6.91077873387739,-0.823245301616172,
5.72937059741184));
#11207=CARTESIAN_POINT('Ctrl Pts',(6.90708649247861,-0.831348026207296,
5.72879830197985));
#11208=CARTESIAN_POINT('Ctrl Pts',(6.90515356855211,-0.835551069460491,
5.72850188585384));
#11209=CARTESIAN_POINT('Ctrl Pts',(6.9004273952516,-0.845734415410518,5.72778471084471));
#11210=CARTESIAN_POINT('Ctrl Pts',(6.89761901927022,-0.851707721478765,
5.72736486917326));
#11211=CARTESIAN_POINT('Ctrl Pts',(6.88757188100193,-0.872804989552912,
5.72588460305805));
#11212=CARTESIAN_POINT('Ctrl Pts',(6.88017190788738,-0.887851991690589,
5.72483356569295));
#11213=CARTESIAN_POINT('Ctrl Pts',(6.86139850173605,-0.924840401948595,
5.72225727555241));
#11214=CARTESIAN_POINT('Ctrl Pts',(6.84980515899305,-0.946667627702199,
5.72074347842823));
#11215=CARTESIAN_POINT('Ctrl Pts',(6.7995002922786,-1.03727285836511,5.71446364953517));
#11216=CARTESIAN_POINT('Ctrl Pts',(6.75712786539693,-1.10394224992717,5.70985072318407));
#11217=CARTESIAN_POINT('Ctrl Pts',(6.61786970184766,-1.296755606723,5.69602177809838));
#11218=CARTESIAN_POINT('Ctrl Pts',(6.50977768791325,-1.41398688631044,5.6868802858042));
#11219=CARTESIAN_POINT('Ctrl Pts',(6.37244728192596,-1.53121770192777,5.67575865074876));
#11220=CARTESIAN_POINT('Ctrl Pts',(6.35573936817078,-1.54501604834893,5.67441390106552));
#11221=CARTESIAN_POINT('Ctrl Pts',(6.32961405947582,-1.56588531880682,5.67232189321447));
#11222=CARTESIAN_POINT('Ctrl Pts',(6.32035295777391,-1.57314988179829,5.67158232804223));
#11223=CARTESIAN_POINT('Ctrl Pts',(6.30451664434112,-1.5853473055098,5.67032081426914));
#11224=CARTESIAN_POINT('Ctrl Pts',(6.29797417142884,-1.5903223189749,5.66980053661757));
#11225=CARTESIAN_POINT('Ctrl Pts',(6.28467472141519,-1.60030633998083,5.66874461955397));
#11226=CARTESIAN_POINT('Ctrl Pts',(6.2779164407825,-1.6053133239208,5.66820891606077));
#11227=CARTESIAN_POINT('Ctrl Pts',(6.26118376894454,-1.61754684892312,5.66688460694955));
#11228=CARTESIAN_POINT('Ctrl Pts',(6.25117382999982,-1.62472395661662,5.66609412351733));
#11229=CARTESIAN_POINT('Ctrl Pts',(6.21365723014178,-1.6511006605735,5.66313747480288));
#11230=CARTESIAN_POINT('Ctrl Pts',(6.18573540341013,-1.66969726008991,5.66094879534436));
#11231=CARTESIAN_POINT('Ctrl Pts',(6.11457381596717,-1.71454410021904,5.65539655748736));
#11232=CARTESIAN_POINT('Ctrl Pts',(6.07078154686166,-1.73986914340071,5.65200238762648));
#11233=CARTESIAN_POINT('Ctrl Pts',(5.92261401824319,-1.81819581469486,5.64060124850046));
#11234=CARTESIAN_POINT('Ctrl Pts',(5.81454417257815,-1.86367557030014,5.63240080369409));
#11235=CARTESIAN_POINT('Ctrl Pts',(5.61737853591381,-1.92692247100687,5.61800530770726));
#11236=CARTESIAN_POINT('Ctrl Pts',(5.52985907899718,-1.94859339585833,5.61180532197608));
#11237=CARTESIAN_POINT('Ctrl Pts',(5.4303822703508,-1.96618364704437,5.60516558673266));
#11238=CARTESIAN_POINT('Ctrl Pts',(5.41958309597748,-1.96800166651936,5.60445014006174));
#11239=CARTESIAN_POINT('Ctrl Pts',(5.40320753022592,-1.97061997079041,5.60337391776093));
#11240=CARTESIAN_POINT('Ctrl Pts',(5.3976420260537,-1.97148568644396,5.60300965692064));
#11241=CARTESIAN_POINT('Ctrl Pts',(5.38762647170969,-1.97300018920297,5.60235694763225));
#11242=CARTESIAN_POINT('Ctrl Pts',(5.38317784866881,-1.97365750887705,5.60206803332873));
#11243=CARTESIAN_POINT('Ctrl Pts',(5.3733993633529,-1.97506858531866,5.60143517234842));
#11244=CARTESIAN_POINT('Ctrl Pts',(5.36806866477218,-1.97581581437817,5.6010915926698));
#11245=CARTESIAN_POINT('Ctrl Pts',(5.35272875676186,-1.97790280350508,5.60010680699909));
#11246=CARTESIAN_POINT('Ctrl Pts',(5.34271214060866,-1.97918817032043,5.59946855567015));
#11247=CARTESIAN_POINT('Ctrl Pts',(5.26998906660551,-1.98795941254316,5.5948666068882));
#11248=CARTESIAN_POINT('Ctrl Pts',(5.20696144904454,-1.99254058791037,5.59104967115456));
#11249=CARTESIAN_POINT('Ctrl Pts',(5.01315043191117,-1.99739909849227,5.5795518448154));
#11250=CARTESIAN_POINT('Ctrl Pts',(4.88247576416099,-1.98782424339013,5.57211387098648));
#11251=CARTESIAN_POINT('Ctrl Pts',(4.66583867661601,-1.95033312945932,5.55918112134196));
#11252=CARTESIAN_POINT('Ctrl Pts',(4.57913235188481,-1.92926405943375,5.55384046060544));
#11253=CARTESIAN_POINT('Ctrl Pts',(4.47919166765882,-1.89776083004868,5.54733725067333));
#11254=CARTESIAN_POINT('Ctrl Pts',(4.46430780380629,-1.8928756734287,5.54635963283881));
#11255=CARTESIAN_POINT('Ctrl Pts',(4.43997107480193,-1.88456913181486,5.5447453734981));
#11256=CARTESIAN_POINT('Ctrl Pts',(4.43048362489725,-1.88125063224838,5.54411210543214));
#11257=CARTESIAN_POINT('Ctrl Pts',(4.41345460695683,-1.87514942623074,5.54296812017506));
#11258=CARTESIAN_POINT('Ctrl Pts',(4.4059039658673,-1.87239254901107,5.54245826602385));
#11259=CARTESIAN_POINT('Ctrl Pts',(4.38982218180117,-1.86641038907222,5.54136666417947));
#11260=CARTESIAN_POINT('Ctrl Pts',(4.38129610798701,-1.86317209221796,5.54078449311225));
#11261=CARTESIAN_POINT('Ctrl Pts',(4.35825309801326,-1.85423880323849,5.53920159560043));
#11262=CARTESIAN_POINT('Ctrl Pts',(4.34378049014782,-1.84843195991956,5.53819715428113));
#11263=CARTESIAN_POINT('Ctrl Pts',(4.26708715046856,-1.81661129765646,5.53281828215199));
#11264=CARTESIAN_POINT('Ctrl Pts',(4.20615404158314,-1.7876270104557,5.52834442298922));
#11265=CARTESIAN_POINT('Ctrl Pts',(4.00332127348718,-1.67821473273237,5.5127494763014));
#11266=CARTESIAN_POINT('Ctrl Pts',(3.86986687261089,-1.58351471368963,5.50119597280198));
#11267=CARTESIAN_POINT('Ctrl Pts',(3.70846355491796,-1.43627035264085,5.48620213325376));
#11268=CARTESIAN_POINT('Ctrl Pts',(3.66905498685675,-1.3971865673288,5.48245079280582));
#11269=CARTESIAN_POINT('Ctrl Pts',(3.62500117812364,-1.34969042795929,5.47819884208006));
#11270=CARTESIAN_POINT('Ctrl Pts',(3.61872621701148,-1.34282956191797,5.47759174798476));
#11271=CARTESIAN_POINT('Ctrl Pts',(3.60863733160063,-1.33164259574499,5.47661365303636));
#11272=CARTESIAN_POINT('Ctrl Pts',(3.60479387937749,-1.32734348245983,5.47624055839702));
#11273=CARTESIAN_POINT('Ctrl Pts',(3.59798093544976,-1.31965599529119,5.47557844303638));
#11274=CARTESIAN_POINT('Ctrl Pts',(3.59500422981552,-1.31627417309262,5.47528889467969));
#11275=CARTESIAN_POINT('Ctrl Pts',(3.58856541483381,-1.30890889940386,5.47466203362447));
#11276=CARTESIAN_POINT('Ctrl Pts',(3.58510764996193,-1.30492178693169,5.47432503748345));
#11277=CARTESIAN_POINT('Ctrl Pts',(3.57540112315549,-1.29363913692636,5.47337785680347));
#11278=CARTESIAN_POINT('Ctrl Pts',(3.56918907613332,-1.28631200257696,5.47277028619838));
#11279=CARTESIAN_POINT('Ctrl Pts',(3.53027013863521,-1.23972890118846,5.46895285777323));
#11280=CARTESIAN_POINT('Ctrl Pts',(3.49902576058154,-1.19926968687474,5.4658385949702));
#11281=CARTESIAN_POINT('Ctrl Pts',(3.38112572229012,-1.03382792794735,5.45368349415277));
#11282=CARTESIAN_POINT('Ctrl Pts',(3.3073270949795,-0.900316487034451,5.44509259584546));
#11283=CARTESIAN_POINT('Ctrl Pts',(3.21844048613116,-0.684518264250985,
5.43131332792379));
#11284=CARTESIAN_POINT('Ctrl Pts',(3.19209974908524,-0.607512118360447,
5.42642266848376));
#11285=CARTESIAN_POINT('Ctrl Pts',(3.1664572208232,-0.51430419075007,5.42042073103093));
#11286=CARTESIAN_POINT('Ctrl Pts',(3.16255280260136,-0.49944270841317,5.41946148457612));
#11287=CARTESIAN_POINT('Ctrl Pts',(3.15640123941935,-0.474876384633146,
5.41787141090199));
#11288=CARTESIAN_POINT('Ctrl Pts',(3.15405436032711,-0.465197010221756,
5.41724378402069));
#11289=CARTESIAN_POINT('Ctrl Pts',(3.14994627097088,-0.44768198884405,5.4161058816988));
#11290=CARTESIAN_POINT('Ctrl Pts',(3.14815969603198,-0.439852464435022,
5.41559642936443));
#11291=CARTESIAN_POINT('Ctrl Pts',(3.14443160680815,-0.423047148392428,
5.41450115248068));
#11292=CARTESIAN_POINT('Ctrl Pts',(3.14250470601428,-0.414068337982984,
5.41391487487658));
#11293=CARTESIAN_POINT('Ctrl Pts',(3.13741467739742,-0.389525381279098,
5.41230919977965));
#11294=CARTESIAN_POINT('Ctrl Pts',(3.13437537952753,-0.37393651955715,5.41128590346255));
#11295=CARTESIAN_POINT('Ctrl Pts',(3.1185842089205,-0.287456119014403,5.40558888371829));
#11296=CARTESIAN_POINT('Ctrl Pts',(3.10949462434862,-0.215958324588518,
5.4008010636791));
#11297=CARTESIAN_POINT('Ctrl Pts',(3.09265206787229,0.0165283067286086,
5.38498452533375));
#11298=CARTESIAN_POINT('Ctrl Pts',(3.10051650234774,0.177985539301892,5.37356500852506));
#11299=CARTESIAN_POINT('Ctrl Pts',(3.13657367484361,0.388519350413989,5.35893076200216));
#11300=CARTESIAN_POINT('Ctrl Pts',(3.14748733273616,0.439944104046039,5.35538353792883));
#11301=CARTESIAN_POINT('Ctrl Pts',(3.16267678199651,0.499769825089018,5.35133333449026));
#11302=CARTESIAN_POINT('Ctrl Pts',(3.16499459449813,0.508641919632829,5.3507347084816));
#11303=CARTESIAN_POINT('Ctrl Pts',(3.16885961096554,0.523029948401436,5.34976753521139));
#11304=CARTESIAN_POINT('Ctrl Pts',(3.17036951024386,0.528555638806814,5.34939696769402));
#11305=CARTESIAN_POINT('Ctrl Pts',(3.17310868553862,0.538412846588221,5.34873757318475));
#11306=CARTESIAN_POINT('Ctrl Pts',(3.17432884120676,0.542746770566812,5.34844823617108));
#11307=CARTESIAN_POINT('Ctrl Pts',(3.17701889960714,0.552179161052406,5.34781979385125));
#11308=CARTESIAN_POINT('Ctrl Pts',(3.17849447269919,0.557275902517075,5.34748101887947));
#11309=CARTESIAN_POINT('Ctrl Pts',(3.18273574494844,0.571709726251058,5.34652373073608));
#11310=CARTESIAN_POINT('Ctrl Pts',(3.18554954915867,0.581032681353897,5.34590792116906));
#11311=CARTESIAN_POINT('Ctrl Pts',(3.20439890485507,0.641871842668362,5.34190350623619));
#11312=CARTESIAN_POINT('Ctrl Pts',(3.22245220902761,0.692744915447949,5.33862164795559));
#11313=CARTESIAN_POINT('Ctrl Pts',(3.30920633196461,0.908953947022581,5.32471425094573));
#11314=CARTESIAN_POINT('Ctrl Pts',(3.39792147487279,1.06535440925857,5.3146837187225));
#11315=CARTESIAN_POINT('Ctrl Pts',(3.53943388099586,1.25135128905305,5.30066396719669));
#11316=CARTESIAN_POINT('Ctrl Pts',(3.5743218737062,1.29349193818094,5.29733057835285));
#11317=CARTESIAN_POINT('Ctrl Pts',(3.62108074417206,1.34546553701348,5.29297954516331));
#11318=CARTESIAN_POINT('Ctrl Pts',(3.63139581736244,1.3566702121026,5.29202651557373));
#11319=CARTESIAN_POINT('Ctrl Pts',(3.64803688835665,1.37433613003269,5.29049911268272));
#11320=CARTESIAN_POINT('Ctrl Pts',(3.65428039951754,1.38087451561727,5.28992825838498));
#11321=CARTESIAN_POINT('Ctrl Pts',(3.66560701718082,1.39257577487941,5.28889646843536));
#11322=CARTESIAN_POINT('Ctrl Pts',(3.67067424258776,1.39775385404223,5.28843622612792));
#11323=CARTESIAN_POINT('Ctrl Pts',(3.68265166352345,1.40986064924029,5.28735143663487));
#11324=CARTESIAN_POINT('Ctrl Pts',(3.68958480950051,1.41676629954124,5.28672588704078));
#11325=CARTESIAN_POINT('Ctrl Pts',(3.70992532846668,1.43673016446754,5.28489733311379));
#11326=CARTESIAN_POINT('Ctrl Pts',(3.72346571649023,1.44965075772637,5.28368842104235));
#11327=CARTESIAN_POINT('Ctrl Pts',(3.83912906095041,1.55695109141519,5.27342807270738));
#11328=CARTESIAN_POINT('Ctrl Pts',(3.95066263302172,1.64058686049391,5.26392182413216));
#11329=CARTESIAN_POINT('Ctrl Pts',(4.18426046130562,1.78029588055611,5.24497833906629));
#11330=CARTESIAN_POINT('Ctrl Pts',(4.30512693710624,1.83704176675259,5.2356107904843));
#11331=CARTESIAN_POINT('Ctrl Pts',(4.44533202950561,1.88645713430267,5.22576750428409));
#11332=CARTESIAN_POINT('Ctrl Pts',(4.45996881529259,1.89142541156067,5.22475210914947));
#11333=CARTESIAN_POINT('Ctrl Pts',(4.48030490032262,1.89806565675324,5.22335956639989));
#11334=CARTESIAN_POINT('Ctrl Pts',(4.48595568860229,1.89988291134891,5.22297455559995));
#11335=CARTESIAN_POINT('Ctrl Pts',(4.49567440435848,1.90296058388496,5.22231580030969));
#11336=CARTESIAN_POINT('Ctrl Pts',(4.49973837143314,1.90423323544996,5.22204135933294));
#11337=CARTESIAN_POINT('Ctrl Pts',(4.50824122589562,1.90686607676153,5.22146934156337));
#11338=CARTESIAN_POINT('Ctrl Pts',(4.51268082488346,1.90822379678429,5.22117191874408));
#11339=CARTESIAN_POINT('Ctrl Pts',(4.52352551970217,1.91149896879319,5.22044834556641));
#11340=CARTESIAN_POINT('Ctrl Pts',(4.52993566868948,1.91339976420366,5.22002315266412));
#11341=CARTESIAN_POINT('Ctrl Pts',(4.55298724124787,1.92010932092578,5.218502678237));
#11342=CARTESIAN_POINT('Ctrl Pts',(4.5696821353629,1.92473366020924,5.21741747241571));
#11343=CARTESIAN_POINT('Ctrl Pts',(4.61139626035668,1.93570506969996,5.2147407512475));
#11344=CARTESIAN_POINT('Ctrl Pts',(4.63648298079526,1.9417852914853,5.21316187996794));
#11345=CARTESIAN_POINT('Ctrl Pts',(4.74473267047711,1.9658071403892,5.20645367954117));
#11346=CARTESIAN_POINT('Ctrl Pts',(4.82888411952969,1.9789067901642,5.20149969730753));
#11347=CARTESIAN_POINT('Ctrl Pts',(5.06300988690219,2.00014466767902,5.18784552468283));
#11348=CARTESIAN_POINT('Ctrl Pts',(5.21343257149962,1.99680167224567,5.17917935503643));
#11349=CARTESIAN_POINT('Ctrl Pts',(5.38648827413168,1.9733182970053,5.16842906757464));
#11350=CARTESIAN_POINT('Ctrl Pts',(5.41085891551759,1.96954979926487,5.16689811242441));
#11351=CARTESIAN_POINT('Ctrl Pts',(5.44483886518325,1.96364838887499,5.16473699090043));
#11352=CARTESIAN_POINT('Ctrl Pts',(5.45451238569607,1.96189458806115,5.16411873839884));
#11353=CARTESIAN_POINT('Ctrl Pts',(5.47222599575718,1.95854769048859,5.16298091078681));
#11354=CARTESIAN_POINT('Ctrl Pts',(5.48027002686475,1.956976403063,5.16246203495747));
#11355=CARTESIAN_POINT('Ctrl Pts',(5.49657754744652,1.95368649505009,5.16140561620808));
#11356=CARTESIAN_POINT('Ctrl Pts',(5.50484026204032,1.95196491305983,5.16086798882051));
#11357=CARTESIAN_POINT('Ctrl Pts',(5.52527221945312,1.94757232000018,5.15953258079778));
#11358=CARTESIAN_POINT('Ctrl Pts',(5.53742770432753,1.94483966595977,5.15873285203241));
#11359=CARTESIAN_POINT('Ctrl Pts',(5.58321642052769,1.93409438480144,5.15569996350098));
#11360=CARTESIAN_POINT('Ctrl Pts',(5.61666334983906,1.9253220534628,5.15344275373732));
#11361=CARTESIAN_POINT('Ctrl Pts',(5.70049141713316,1.9009905661415,5.14767583470599));
#11362=CARTESIAN_POINT('Ctrl Pts',(5.75051269653897,1.8842956181932,5.14413239413984));
#11363=CARTESIAN_POINT('Ctrl Pts',(5.88471487483561,1.83351169718912,5.1343542243994));
#11364=CARTESIAN_POINT('Ctrl Pts',(5.96732140419943,1.79562641506956,5.12803060411832));
#11365=CARTESIAN_POINT('Ctrl Pts',(6.1389545685334,1.70225765673671,5.11440966658794));
#11366=CARTESIAN_POINT('Ctrl Pts',(6.22678803790127,1.64510679896248,5.10713048330254));
#11367=CARTESIAN_POINT('Ctrl Pts',(6.32267230170687,1.57137943306154,5.09911238102685));
#11368=CARTESIAN_POINT('Ctrl Pts',(6.33548329912968,1.56127632974721,5.09803970376784));
#11369=CARTESIAN_POINT('Ctrl Pts',(6.35339295260509,1.54679238961031,5.09653982204586));
#11370=CARTESIAN_POINT('Ctrl Pts',(6.35859524052958,1.54254153526504,5.09610411086431));
#11371=CARTESIAN_POINT('Ctrl Pts',(6.36732535362666,1.53533419342582,5.09537301605208));
#11372=CARTESIAN_POINT('Ctrl Pts',(6.37086457140157,1.53239165555807,5.09507665188825));
#11373=CARTESIAN_POINT('Ctrl Pts',(6.3780167456839,1.5264032849146,5.09447785158997));
#11374=CARTESIAN_POINT('Ctrl Pts',(6.38162910761804,1.52335682785821,5.0941754633614));
#11375=CARTESIAN_POINT('Ctrl Pts',(6.39057964103947,1.51575387514746,5.09342624390475));
#11376=CARTESIAN_POINT('Ctrl Pts',(6.39590470538112,1.51118194681546,5.09298052115921));
#11377=CARTESIAN_POINT('Ctrl Pts',(6.4075793589996,1.50105094067484,5.09200307914271));
#11378=CARTESIAN_POINT('Ctrl Pts',(6.41391805892647,1.49547945190704,5.091472222558));
#11379=CARTESIAN_POINT('Ctrl Pts',(6.43216651201427,1.47923328423941,5.0899428246219));
#11380=CARTESIAN_POINT('Ctrl Pts',(6.44398376534353,1.46845514255627,5.08895102906392));
#11381=CARTESIAN_POINT('Ctrl Pts',(6.48487159682627,1.43025174078433,5.08550910875932));
#11382=CARTESIAN_POINT('Ctrl Pts',(6.51324801847542,1.40209467902018,5.08310174116355));
#11383=CARTESIAN_POINT('Ctrl Pts',(6.59893997211107,1.31179509003635,5.07569934300571));
#11384=CARTESIAN_POINT('Ctrl Pts',(6.65316650157718,1.246849269565,5.07081595364142));
#11385=CARTESIAN_POINT('Ctrl Pts',(6.77813840689327,1.07621829823807,5.05853390122981));
#11386=CARTESIAN_POINT('Ctrl Pts',(6.84320421747374,0.966863426912216,5.05111615554143));
#11387=CARTESIAN_POINT('Ctrl Pts',(6.90804047792998,0.829622892047224,5.04177950168581));
#11388=CARTESIAN_POINT('Ctrl Pts',(6.91822656910962,0.80697634255003,5.04023893836912));
#11389=CARTESIAN_POINT('Ctrl Pts',(6.93196804001188,0.774834313478809,5.03804986948117));
#11390=CARTESIAN_POINT('Ctrl Pts',(6.93587810250327,0.765492277738563,5.03741332506443));
#11391=CARTESIAN_POINT('Ctrl Pts',(6.94256793925524,0.749160632058954,5.03629982655155));
#11392=CARTESIAN_POINT('Ctrl Pts',(6.94537965374703,0.742184264096279,5.03582395471267));
#11393=CARTESIAN_POINT('Ctrl Pts',(6.95118551398956,0.72754054335906,5.03482453616651));
#11394=CARTESIAN_POINT('Ctrl Pts',(6.95417178665268,0.719870241154159,5.03430073711077));
#11395=CARTESIAN_POINT('Ctrl Pts',(6.96117796504693,0.701539955500313,5.03304813347918));
#11396=CARTESIAN_POINT('Ctrl Pts',(6.96515415114846,0.690863677980075,5.03231789168681));
#11397=CARTESIAN_POINT('Ctrl Pts',(6.97839078583096,0.654369759003233,5.02981912231209));
#11398=CARTESIAN_POINT('Ctrl Pts',(6.987209766122,0.62839639111193,5.02803617675052));
#11399=CARTESIAN_POINT('Ctrl Pts',(7.00715074819199,0.565430851827448,5.02370100643216));
#11400=CARTESIAN_POINT('Ctrl Pts',(7.0177389223077,0.528282505822011,5.02113267654849));
#11401=CARTESIAN_POINT('Ctrl Pts',(7.06797965083055,0.330389628924655,5.00739592710424));
#11402=CARTESIAN_POINT('Ctrl Pts',(7.08857715545311,0.165496289135984,4.99568651530648));
#11403=CARTESIAN_POINT('Ctrl Pts',(7.08857715545311,-3.14833228931555E-12,
4.98428615635939));
#11404=CARTESIAN_POINT('Ctrl Pts',(7.08857715545311,4.63564351804039E-12,
4.82758772788682));
#11405=CARTESIAN_POINT('Ctrl Pts',(7.08857715545311,0.000573719257101207,
4.82762772343443));
#11406=CARTESIAN_POINT('Ctrl Pts',(7.08857690794847,0.00114744551234271,
4.82766771905986));
#11407=CARTESIAN_POINT('Ctrl Pts',(7.08848669692276,0.105696976420473,4.83495600109056));
#11408=CARTESIAN_POINT('Ctrl Pts',(7.08026752389154,0.209517214713461,4.84218852636164));
#11409=CARTESIAN_POINT('Ctrl Pts',(7.06143895786786,0.328324282050292,4.85016246565267));
#11410=CARTESIAN_POINT('Ctrl Pts',(7.05869142249721,0.344385673291137,4.85123375556096));
#11411=CARTESIAN_POINT('Ctrl Pts',(7.05453410036983,0.367016244780663,4.85273204744083));
#11412=CARTESIAN_POINT('Ctrl Pts',(7.05328755320094,0.37361424031373,4.85316753250585));
#11413=CARTESIAN_POINT('Ctrl Pts',(7.05113055114468,0.384723481699219,4.85389835853669));
#11414=CARTESIAN_POINT('Ctrl Pts',(7.05023776506502,0.389238061165263,4.85419467843257));
#11415=CARTESIAN_POINT('Ctrl Pts',(7.04837726814135,0.398477958442519,4.85479971565694));
#11416=CARTESIAN_POINT('Ctrl Pts',(7.04740803109899,0.403202914030322,4.85510834512106));
#11417=CARTESIAN_POINT('Ctrl Pts',(7.04487923215159,0.415307410094315,4.8558971441728));
#11418=CARTESIAN_POINT('Ctrl Pts',(7.04329491966233,0.422681785173675,4.8563759308144));
#11419=CARTESIAN_POINT('Ctrl Pts',(7.03654529535589,0.453253315835352,4.85835412275427));
#11420=CARTESIAN_POINT('Ctrl Pts',(7.03100723390141,0.476367295760992,4.85983375012937));
#11421=CARTESIAN_POINT('Ctrl Pts',(7.01507214287535,0.537992613721132,4.86374908972714));
#11422=CARTESIAN_POINT('Ctrl Pts',(7.00393062331271,0.576301561377695,4.86615187004281));
#11423=CARTESIAN_POINT('Ctrl Pts',(6.96302692821696,0.702679239000464,4.87405110996139));
#11424=CARTESIAN_POINT('Ctrl Pts',(6.92826017460389,0.789001306990145,4.87940605376871));
#11425=CARTESIAN_POINT('Ctrl Pts',(6.83068644838862,0.989582887833457,4.89237094102702));
#11426=CARTESIAN_POINT('Ctrl Pts',(6.76247293580302,1.100713112585,4.90001172681703));
#11427=CARTESIAN_POINT('Ctrl Pts',(6.67414691277301,1.21732481932324,4.90908359471025));
#11428=CARTESIAN_POINT('Ctrl Pts',(6.66420405686953,1.23012463374942,4.91009451936571));
#11429=CARTESIAN_POINT('Ctrl Pts',(6.64774200029192,1.25079197769677,4.91175256753217));
#11430=CARTESIAN_POINT('Ctrl Pts',(6.64131625956643,1.2587332453353,4.91239599353068));
#11431=CARTESIAN_POINT('Ctrl Pts',(6.62971568124969,1.27284675754089,4.91355110007175));
#11432=CARTESIAN_POINT('Ctrl Pts',(6.62456388791828,1.27903771822497,4.91406184567603));
#11433=CARTESIAN_POINT('Ctrl Pts',(6.61356523961786,1.29209327232376,4.91514763942081));
#11434=CARTESIAN_POINT('Ctrl Pts',(6.60770906364544,1.2989497421019,4.9157230611546));
#11435=CARTESIAN_POINT('Ctrl Pts',(6.59190775368478,1.3171980718919,4.91726865015813));
#11436=CARTESIAN_POINT('Ctrl Pts',(6.58187938420923,1.32851676055405,4.91824223920823));
#11437=CARTESIAN_POINT('Ctrl Pts',(6.53092555234893,1.38472587740811,4.9231537752426));
#11438=CARTESIAN_POINT('Ctrl Pts',(6.48809711819846,1.42784016355731,4.92717160452332));
#11439=CARTESIAN_POINT('Ctrl Pts',(6.34890589818336,1.55571883139408,4.93990797492455));
#11440=CARTESIAN_POINT('Ctrl Pts',(6.24629614124813,1.63318466892481,4.94887778886495));
#11441=CARTESIAN_POINT('Ctrl Pts',(6.05475850589738,1.75069776380793,4.96451882559785));
#11442=CARTESIAN_POINT('Ctrl Pts',(5.96898029257621,1.79511645302358,4.97118013028009));
#11443=CARTESIAN_POINT('Ctrl Pts',(5.8702516617401,1.83747448139454,4.97824127769598));
#11444=CARTESIAN_POINT('Ctrl Pts',(5.86015226828568,1.84170934680892,4.97895673789953));
#11445=CARTESIAN_POINT('Ctrl Pts',(5.84480627712942,1.84799611603437,4.98003297649632));
#11446=CARTESIAN_POINT('Ctrl Pts',(5.8395852140434,1.8501092416391,4.98039724025271));
#11447=CARTESIAN_POINT('Ctrl Pts',(5.83017962832406,1.85386968812512,4.98104995264498));
#11448=CARTESIAN_POINT('Ctrl Pts',(5.82599844271205,1.85552499097945,4.98133886715646));
#11449=CARTESIAN_POINT('Ctrl Pts',(5.81680013763755,1.85913060401638,4.98197172609797));
#11450=CARTESIAN_POINT('Ctrl Pts',(5.81178071420334,1.86107474994281,4.98231530354701));
#11451=CARTESIAN_POINT('Ctrl Pts',(5.79732220399448,1.86660768574782,4.9833000762067));
#11452=CARTESIAN_POINT('Ctrl Pts',(5.78786349236886,1.87014521065981,4.98393831687609));
#11453=CARTESIAN_POINT('Ctrl Pts',(5.71906665149869,1.89528113580518,4.98853994125855));
#11454=CARTESIAN_POINT('Ctrl Pts',(5.65875303971482,1.91412525036457,4.99235658680572));
#11455=CARTESIAN_POINT('Ctrl Pts',(5.47119892407446,1.96308304804697,5.00385247749157));
#11456=CARTESIAN_POINT('Ctrl Pts',(5.34181666355457,1.98358474727842,5.01128890389283));
#11457=CARTESIAN_POINT('Ctrl Pts',(5.1223381643693,1.99653855049845,5.02422166087855));
#11458=CARTESIAN_POINT('Ctrl Pts',(5.03308009599025,1.99581711373973,5.02956412415536));
#11459=CARTESIAN_POINT('Ctrl Pts',(4.92855463808832,1.98795321375761,5.03606934305721));
#11460=CARTESIAN_POINT('Ctrl Pts',(4.91294756484843,1.98659395373497,5.03704702782196));
#11461=CARTESIAN_POINT('Ctrl Pts',(4.8873559147632,1.98406104247023,5.03866137529451));
#11462=CARTESIAN_POINT('Ctrl Pts',(4.87736114625361,1.98299547513656,5.03929466392463));
#11463=CARTESIAN_POINT('Ctrl Pts',(4.85938871986587,1.98094189613123,5.04043867156936));
#11464=CARTESIAN_POINT('Ctrl Pts',(4.85140812304315,1.97998110737837,5.04094852739906));
#11465=CARTESIAN_POINT('Ctrl Pts',(4.83438564732956,1.97782730369345,5.04204011674125));
#11466=CARTESIAN_POINT('Ctrl Pts',(4.82534573307707,1.97662046449783,5.0426222735232));
#11467=CARTESIAN_POINT('Ctrl Pts',(4.80087323803033,1.97318237989198,5.04420509161456));
#11468=CARTESIAN_POINT('Ctrl Pts',(4.78545828402121,1.97083213855456,5.04520946716294));
#11469=CARTESIAN_POINT('Ctrl Pts',(4.70354266184363,1.95735831959495,5.05058727486061));
#11470=CARTESIAN_POINT('Ctrl Pts',(4.63761737715697,1.9430502977452,5.05506008814791));
#11471=CARTESIAN_POINT('Ctrl Pts',(4.41527720522925,1.88285549072507,5.07064701610538));
#11472=CARTESIAN_POINT('Ctrl Pts',(4.26381972627475,1.8211678573861,5.08219293059166));
#11473=CARTESIAN_POINT('Ctrl Pts',(4.07304397351016,1.71467742696865,5.09718826647046));
#11474=CARTESIAN_POINT('Ctrl Pts',(4.02565914161774,1.68556675578075,5.1009472434908));
#11475=CARTESIAN_POINT('Ctrl Pts',(3.97183278668838,1.64931583519805,5.10520671719149));
#11476=CARTESIAN_POINT('Ctrl Pts',(3.96415374596918,1.64406571755524,5.10581411333155));
#11477=CARTESIAN_POINT('Ctrl Pts',(3.95177297190206,1.63547334838524,5.10679259763656));
#11478=CARTESIAN_POINT('Ctrl Pts',(3.94704862021085,1.63216415368232,5.10716578223072));
#11479=CARTESIAN_POINT('Ctrl Pts',(3.93865971602439,1.62623370020206,5.10782799489912));
#11480=CARTESIAN_POINT('Ctrl Pts',(3.93498962880865,1.62362047566312,5.10811755123467));
#11481=CARTESIAN_POINT('Ctrl Pts',(3.92704043991007,1.61791970280442,5.10874435801259));
#11482=CARTESIAN_POINT('Ctrl Pts',(3.92276472743715,1.61482760551296,5.10908129237846));
#11483=CARTESIAN_POINT('Ctrl Pts',(3.91074375715549,1.60606146107707,5.11002812253459));
#11484=CARTESIAN_POINT('Ctrl Pts',(3.90302699910572,1.60034831847765,5.1106354074763));
#11485=CARTESIAN_POINT('Ctrl Pts',(3.85458264159906,1.56393785663435,5.11444660358583));
#11486=CARTESIAN_POINT('Ctrl Pts',(3.81499989376728,1.5317409676805,5.11755528027043));
#11487=CARTESIAN_POINT('Ctrl Pts',(3.66307025707052,1.39816017047473,5.12966040661471));
#11488=CARTESIAN_POINT('Ctrl Pts',(3.56117802808255,1.28565533322423,5.13821081917022));
#11489=CARTESIAN_POINT('Ctrl Pts',(3.42511921671253,1.09598526195555,5.15198682669929));
#11490=CARTESIAN_POINT('Ctrl Pts',(3.38142821501397,1.02638071854155,5.15692322378292));
#11491=CARTESIAN_POINT('Ctrl Pts',(3.33478599823343,0.940765062971582,5.16297612776706));
#11492=CARTESIAN_POINT('Ctrl Pts',(3.32757604994052,0.927157865778961,5.16393743197347));
#11493=CARTESIAN_POINT('Ctrl Pts',(3.31595885969982,0.90460559798098,5.16553021580144));
#11494=CARTESIAN_POINT('Ctrl Pts',(3.3114597793325,0.89570837647937,5.16615847589545));
#11495=CARTESIAN_POINT('Ctrl Pts',(3.30345716701127,0.879583636267798,5.16729705748947));
#11496=CARTESIAN_POINT('Ctrl Pts',(3.29993020862832,0.872367932585918,5.16780655139943));
#11497=CARTESIAN_POINT('Ctrl Pts',(3.29246729917109,0.856863133478572,5.16890139866501));
#11498=CARTESIAN_POINT('Ctrl Pts',(3.28854478756427,0.848567810433568,5.16948720166505));
#11499=CARTESIAN_POINT('Ctrl Pts',(3.27800372110959,0.825871662698205,5.17109024042847));
#11500=CARTESIAN_POINT('Ctrl Pts',(3.27149945132605,0.811418796162326,5.17211135352792));
#11501=CARTESIAN_POINT('Ctrl Pts',(3.2366143682867,0.731366474942204,5.17777007852239));
#11502=CARTESIAN_POINT('Ctrl Pts',(3.21160610153351,0.664362914660169,5.18251996210409));
#11503=CARTESIAN_POINT('Ctrl Pts',(3.13071396009952,0.406072623288723,5.20087951253324));
#11504=CARTESIAN_POINT('Ctrl Pts',(3.09999535566019,0.208160048299562,5.21517801258646));
#11505=CARTESIAN_POINT('Ctrl Pts',(3.09900529884054,-0.0114417586268873,
5.22981424448838));
#11506=CARTESIAN_POINT('Ctrl Pts',(3.09922718580167,-0.0318777711936141,
5.23116315961155));
#11507=CARTESIAN_POINT('Ctrl Pts',(3.09995626350637,-0.0596715369501025,
5.2329767035658));
#11508=CARTESIAN_POINT('Ctrl Pts',(3.10019022271175,-0.0670343984942129,
5.23345512036498));
#11509=CARTESIAN_POINT('Ctrl Pts',(3.1006256754827,-0.0787019057856752,
5.23420987584505));
#11510=CARTESIAN_POINT('Ctrl Pts',(3.10080033609171,-0.0830073966191989,
5.23448766587285));
#11511=CARTESIAN_POINT('Ctrl Pts',(3.10119044618907,-0.0919113652062631,
5.2350605998534));
#11512=CARTESIAN_POINT('Ctrl Pts',(3.10140786360553,-0.0965096888198008,
5.23535562096739));
#11513=CARTESIAN_POINT('Ctrl Pts',(3.10196949429675,-0.107575885532921,
5.23606361356053));
#11514=CARTESIAN_POINT('Ctrl Pts',(3.10232929867243,-0.114042986133909,
5.23647572527738));
#11515=CARTESIAN_POINT('Ctrl Pts',(3.1036865249775,-0.136467844747534,5.23789939891494));
#11516=CARTESIAN_POINT('Ctrl Pts',(3.10484433154464,-0.152415766437448,
5.23890249934234));
#11517=CARTESIAN_POINT('Ctrl Pts',(3.11306995331485,-0.249532804671289,
5.24496318374307));
#11518=CARTESIAN_POINT('Ctrl Pts',(3.12491439625332,-0.330229119892889,
5.24979673567846));
#11519=CARTESIAN_POINT('Ctrl Pts',(3.16927041597079,-0.54143367631716,5.26242333219809));
#11520=CARTESIAN_POINT('Ctrl Pts',(3.21008188501042,-0.669755414624781,
5.27009147803214));
#11521=CARTESIAN_POINT('Ctrl Pts',(3.28779897839909,-0.849136199244131,
5.2817676140239));
#11522=CARTESIAN_POINT('Ctrl Pts',(3.31468648912195,-0.904116948512592,
5.2854838992962));
#11523=CARTESIAN_POINT('Ctrl Pts',(3.35154438108733,-0.971453322727717,
5.29025782289212));
#11524=CARTESIAN_POINT('Ctrl Pts',(3.35919318010695,-0.98504607710563,5.29123322526791));
#11525=CARTESIAN_POINT('Ctrl Pts',(3.37161103414365,-1.00652075258717,5.29279366562318));
#11526=CARTESIAN_POINT('Ctrl Pts',(3.37627674951127,-1.01446192257436,5.29337499424073));
#11527=CARTESIAN_POINT('Ctrl Pts',(3.38511186516823,-1.02926384820683,5.2944667611415));
#11528=CARTESIAN_POINT('Ctrl Pts',(3.38926802650402,-1.03613232037234,5.29497671156523));
#11529=CARTESIAN_POINT('Ctrl Pts',(3.39865347031188,-1.05143339875253,5.29612033991878));
#11530=CARTESIAN_POINT('Ctrl Pts',(3.40390440985147,-1.05985240616255,5.29675480150723));
#11531=CARTESIAN_POINT('Ctrl Pts',(3.4195983574244,-1.08460187604915,5.29863560582476));
#11532=CARTESIAN_POINT('Ctrl Pts',(3.430216595198,-1.10081931199353,5.29988838397706));
#11533=CARTESIAN_POINT('Ctrl Pts',(3.51810027325618,-1.23086961571095,5.3101040733299));
#11534=CARTESIAN_POINT('Ctrl Pts',(3.60670284975215,-1.33656400974577,5.31951011421758));
#11535=CARTESIAN_POINT('Ctrl Pts',(3.80141070555066,-1.52530226383815,5.33838164596255));
#11536=CARTESIAN_POINT('Ctrl Pts',(3.90647946539576,-1.60844591030783,5.34778283294266));
#11537=CARTESIAN_POINT('Ctrl Pts',(4.03205134424048,-1.68875597179244,5.35765168775827));
#11538=CARTESIAN_POINT('Ctrl Pts',(4.0451178311414,-1.69690111473951,5.35866309905567));
#11539=CARTESIAN_POINT('Ctrl Pts',(4.06334363836582,-1.70797143251194,5.36005115918856));
#11540=CARTESIAN_POINT('Ctrl Pts',(4.06842326122865,-1.7110258762293,5.3604356056916));
#11541=CARTESIAN_POINT('Ctrl Pts',(4.07717383709986,-1.71623474749747,5.36109364991638));
#11542=CARTESIAN_POINT('Ctrl Pts',(4.08083817431937,-1.71840012894711,5.36136794084873));
#11543=CARTESIAN_POINT('Ctrl Pts',(4.08851556189541,-1.72290386676248,5.36193993376229));
#11544=CARTESIAN_POINT('Ctrl Pts',(4.09252988387002,-1.72523995685392,5.36223748030058));
#11545=CARTESIAN_POINT('Ctrl Pts',(4.10235163576087,-1.73090978837254,5.36296182860558));
#11546=CARTESIAN_POINT('Ctrl Pts',(4.1081678316498,-1.73422838810453,5.36338766802693));
#11547=CARTESIAN_POINT('Ctrl Pts',(4.12914829898174,-1.74605975904956,5.36491305902834));
#11548=CARTESIAN_POINT('Ctrl Pts',(4.14440753268719,-1.75440371820867,5.36600244892579));
#11549=CARTESIAN_POINT('Ctrl Pts',(4.18269937689515,-1.77469627757084,5.36869153897599));
#11550=CARTESIAN_POINT('Ctrl Pts',(4.20586017025401,-1.78639734336619,5.37027844413264));
#11551=CARTESIAN_POINT('Ctrl Pts',(4.30661741675954,-1.83485691438885,5.37704108281297));
#11552=CARTESIAN_POINT('Ctrl Pts',(4.38631915362615,-1.86703876795166,5.38203854311386));
#11553=CARTESIAN_POINT('Ctrl Pts',(4.60923548360172,-1.94071411020311,5.39567334601262));
#11554=CARTESIAN_POINT('Ctrl Pts',(4.75538865892204,-1.97145979331053,5.40428070599617));
#11555=CARTESIAN_POINT('Ctrl Pts',(4.92819698062149,-1.98801534501321,5.41496622959319));
#11556=CARTESIAN_POINT('Ctrl Pts',(4.95283958021462,-1.98991476875213,5.41650056308381));
#11557=CARTESIAN_POINT('Ctrl Pts',(4.98733357024458,-1.9919295933272,5.41866566577576));
#11558=CARTESIAN_POINT('Ctrl Pts',(4.99716081289375,-1.99243067662212,5.41928446153285));
#11559=CARTESIAN_POINT('Ctrl Pts',(5.01518176750561,-1.99321591350688,5.42042297107007));
#11560=CARTESIAN_POINT('Ctrl Pts',(5.02337433408403,-1.99352230276203,5.42094198238258));
#11561=CARTESIAN_POINT('Ctrl Pts',(5.04000160084478,-1.99404151396235,5.42199834563052));
#11562=CARTESIAN_POINT('Ctrl Pts',(5.04843622069285,-1.99425134052624,5.4225357800192));
#11563=CARTESIAN_POINT('Ctrl Pts',(5.06931433635182,-1.99463820121408,5.42387007832624));
#11564=CARTESIAN_POINT('Ctrl Pts',(5.08175850535056,-1.99475230746542,5.42466888331444));
#11565=CARTESIAN_POINT('Ctrl Pts',(5.12867284228941,-1.9947434750988,5.42769407472404));
#11566=CARTESIAN_POINT('Ctrl Pts',(5.16313511938344,-1.99384350320989,5.4299443536146));
#11567=CARTESIAN_POINT('Ctrl Pts',(5.2499826175256,-1.98932127430707,5.43568943326603));
#11568=CARTESIAN_POINT('Ctrl Pts',(5.30227789606448,-1.98452290892568,5.43921763996204));
#11569=CARTESIAN_POINT('Ctrl Pts',(5.45861817953614,-1.96393024284312,5.44996168642467));
#11570=CARTESIAN_POINT('Ctrl Pts',(5.56166039276611,-1.9419638435852,5.4573161005389));
#11571=CARTESIAN_POINT('Ctrl Pts',(5.75719993620534,-1.88380715312217,5.4715205431783));
#11572=CARTESIAN_POINT('Ctrl Pts',(5.84970623669408,-1.84863307327996,5.47835207330984));
#11573=CARTESIAN_POINT('Ctrl Pts',(5.94910254938537,-1.80212383121095,5.48556420722634));
#11574=CARTESIAN_POINT('Ctrl Pts',(5.95893455942866,-1.79742468404907,5.48627608306903));
#11575=CARTESIAN_POINT('Ctrl Pts',(5.97377911412428,-1.79017979712449,5.48734801468233));
#11576=CARTESIAN_POINT('Ctrl Pts',(5.97882003274639,-1.78769314050534,5.48771151537912));
#11577=CARTESIAN_POINT('Ctrl Pts',(5.98787450052443,-1.78317893809211,5.48836342997736));
#11578=CARTESIAN_POINT('Ctrl Pts',(5.99189174453633,-1.78115911009823,5.48865230438652));
#11579=CARTESIAN_POINT('Ctrl Pts',(5.99591982727087,-1.77911673994173,5.48894159134309));
#11580=CARTESIAN_POINT('Ctrl Pts',(5.99593739984907,-1.77910782974053,5.48894285335541));
#11581=CARTESIAN_POINT('Ctrl Pts',(5.99597231062825,-1.77909012752922,5.48894536053409));
#11582=CARTESIAN_POINT('Ctrl Pts',(5.99598964882855,-1.77908133552812,5.4889466057006));
#11583=CARTESIAN_POINT('Ctrl Pts',(5.99602409448578,-1.7790638679002,5.4889490794492));
#11584=CARTESIAN_POINT('Ctrl Pts',(5.99604120190241,-1.77905519230222,5.48895030802856));
#11585=CARTESIAN_POINT('Ctrl Pts',(5.99607518929048,-1.7790379558331,5.48895274884028));
#11586=CARTESIAN_POINT('Ctrl Pts',(5.99609206933451,-1.77902939493332,5.488953961078));
#11587=CARTESIAN_POINT('Ctrl Pts',(5.99612560553281,-1.77901238608183,5.48895636946228));
#11588=CARTESIAN_POINT('Ctrl Pts',(5.99614226165779,-1.77900393815293,5.48895756560689));
#11589=CARTESIAN_POINT('Ctrl Pts',(5.99617535341753,-1.77898715354271,5.48895994204957));
#11590=CARTESIAN_POINT('Ctrl Pts',(5.99619178901208,-1.77897881688951,5.48896112234492));
#11591=CARTESIAN_POINT('Ctrl Pts',(5.9962244429254,-1.77896225322332,5.4889634673204));
#11592=CARTESIAN_POINT('Ctrl Pts',(5.99624066126477,-1.77895402620737,5.48896463200216));
#11593=CARTESIAN_POINT('Ctrl Pts',(5.99627288399326,-1.77893768015119,5.48896694598978));
#11594=CARTESIAN_POINT('Ctrl Pts',(5.99628888836769,-1.7789295611257,5.48896809529472));
#11595=CARTESIAN_POINT('Ctrl Pts',(5.99632068622825,-1.77891342951889,5.48897037874903));
#11596=CARTESIAN_POINT('Ctrl Pts',(5.9963364797822,-1.77890541691027,5.48897151290341));
#11597=CARTESIAN_POINT('Ctrl Pts',(5.99636785921738,-1.77888949652702,5.48897376628796));
#11598=CARTESIAN_POINT('Ctrl Pts',(5.99638344509576,-1.77888158876074,5.48897488551807));
#11599=CARTESIAN_POINT('Ctrl Pts',(5.99641441239506,-1.77886587645148,5.48897710928539));
#11600=CARTESIAN_POINT('Ctrl Pts',(5.99642979375325,-1.77885807194704,5.48897821381824));
#11601=CARTESIAN_POINT('Ctrl Pts',(5.99646035482178,-1.77884256475587,5.48898040839322));
#11602=CARTESIAN_POINT('Ctrl Pts',(5.99647553461199,-1.77883486203515,5.48898149844123));
#11603=CARTESIAN_POINT('Ctrl Pts',(5.9965056956834,-1.77881955683817,5.48898366427235));
#11604=CARTESIAN_POINT('Ctrl Pts',(5.99652067693711,-1.77881195438221,5.48898474005361));
#11605=CARTESIAN_POINT('Ctrl Pts',(5.99655044380506,-1.7787968482775,5.48898687755769));
#11606=CARTESIAN_POINT('Ctrl Pts',(5.9965652294263,-1.77878934463137,5.48898793928114));
#11607=CARTESIAN_POINT('Ctrl Pts',(5.99659460802554,-1.77877443464417,5.48899004888513));
#11608=CARTESIAN_POINT('Ctrl Pts',(5.99660920095602,-1.77876702833322,5.48899109676238));
#11609=CARTESIAN_POINT('Ctrl Pts',(5.99663819683887,-1.77875231168166,5.48899317886573));
#11610=CARTESIAN_POINT('Ctrl Pts',(5.99665259986189,-1.77874500131103,5.48899421309703));
#11611=CARTESIAN_POINT('Ctrl Pts',(5.99668121873968,-1.77873047513138,5.4889962681106));
#11612=CARTESIAN_POINT('Ctrl Pts',(5.99669543462644,-1.77872325931179,5.48899728889529));
#11613=CARTESIAN_POINT('Ctrl Pts',(5.99672368212086,-1.77870892078466,5.48899931722346));
#11614=CARTESIAN_POINT('Ctrl Pts',(5.99673771367204,-1.77870179811131,5.489000324763));
#11615=CARTESIAN_POINT('Ctrl Pts',(5.99676559505476,-1.7786876445939,5.48900232678501));
#11616=CARTESIAN_POINT('Ctrl Pts',(5.99677944492023,-1.77868061373799,5.48900332127002));
#11617=CARTESIAN_POINT('Ctrl Pts',(5.99680696561645,-1.77866664250849,5.48900529737609));
#11618=CARTESIAN_POINT('Ctrl Pts',(5.99682063643611,-1.77865970214577,5.48900627899647));
#11619=CARTESIAN_POINT('Ctrl Pts',(5.99684780177849,-1.77864591052832,5.48900822957017));
#11620=CARTESIAN_POINT('Ctrl Pts',(5.99686129621501,-1.77863905932245,5.48900919851742));
#11621=CARTESIAN_POINT('Ctrl Pts',(5.99688811124726,-1.77862544478689,5.48901112392156));
#11622=CARTESIAN_POINT('Ctrl Pts',(5.99690143185286,-1.77861868145712,5.48901208037926));
#11623=CARTESIAN_POINT('Ctrl Pts',(5.99692790160734,-1.77860524147804,5.4890139809758));
#11624=CARTESIAN_POINT('Ctrl Pts',(5.99694105083226,-1.77859856479493,5.48901492512019));
#11625=CARTESIAN_POINT('Ctrl Pts',(5.99696718052759,-1.77858529675144,5.48901680128443));
#11626=CARTESIAN_POINT('Ctrl Pts',(5.99698016093245,-1.77857870542902,5.48901773329967));
#11627=CARTESIAN_POINT('Ctrl Pts',(5.99700595525111,-1.77856560697152,5.48901958536842));
#11628=CARTESIAN_POINT('Ctrl Pts',(5.99701876920665,-1.7785590998198,5.48902050542503));
#11629=CARTESIAN_POINT('Ctrl Pts',(5.99704423317913,-1.7785461684211,5.48902233376005));
#11630=CARTESIAN_POINT('Ctrl Pts',(5.99705688314776,-1.77853974420308,5.4890232420351));
#11631=CARTESIAN_POINT('Ctrl Pts',(5.99708289483485,-1.77852653395965,5.48902510968199));
#11632=CARTESIAN_POINT('Ctrl Pts',(5.99709625660383,-1.77851974788894,5.48902606905706));
#11633=CARTESIAN_POINT('Ctrl Pts',(6.0020071055388,-1.77602559473077,5.48937866658172));
#11634=CARTESIAN_POINT('Ctrl Pts',(6.00689436806657,-1.77351797336801,5.48972904182116));
#11635=CARTESIAN_POINT('Ctrl Pts',(6.0213078336732,-1.7660471492128,5.49076098323373));
#11636=CARTESIAN_POINT('Ctrl Pts',(6.03080455503388,-1.76102706011105,5.49143911571422));
#11637=CARTESIAN_POINT('Ctrl Pts',(6.0526105316357,-1.74927380163278,5.49299314230048));
#11638=CARTESIAN_POINT('Ctrl Pts',(6.06489036143997,-1.74248692086713,5.49386599515891));
#11639=CARTESIAN_POINT('Ctrl Pts',(6.20517424038399,-1.66301045399931,5.50382292478515));
#11640=CARTESIAN_POINT('Ctrl Pts',(6.32484238670365,-1.57648637434162,5.51220221617603));
#11641=CARTESIAN_POINT('Ctrl Pts',(6.52236952541922,-1.39733901816774,5.52773127436068));
#11642=CARTESIAN_POINT('Ctrl Pts',(6.60343485634565,-1.30933903869002,5.53478130645898));
#11643=CARTESIAN_POINT('Ctrl Pts',(6.68606044956264,-1.20170136284439,5.54319530638623));
#11644=CARTESIAN_POINT('Ctrl Pts',(6.6958225566121,-1.18865627435675,5.54421147237901));
#11645=CARTESIAN_POINT('Ctrl Pts',(6.71145855825071,-1.16721938263567,5.54587640405648));
#11646=CARTESIAN_POINT('Ctrl Pts',(6.71742966952308,-1.15889918136026,5.54652142002283));
#11647=CARTESIAN_POINT('Ctrl Pts',(6.72798343430515,-1.14395180522961,5.54767828501758));
#11648=CARTESIAN_POINT('Ctrl Pts',(6.73259053399238,-1.13734210440813,5.54818918784432));
#11649=CARTESIAN_POINT('Ctrl Pts',(6.74226003692117,-1.12328875699047,5.54927415805731));
#11650=CARTESIAN_POINT('Ctrl Pts',(6.74731233500627,-1.1158384080682,5.54984859162818));
#11651=CARTESIAN_POINT('Ctrl Pts',(6.76067802194942,-1.09583865062556,5.55138872870582));
#11652=CARTESIAN_POINT('Ctrl Pts',(6.76889994529216,-1.08322910206195,5.55235781200575));
#11653=CARTESIAN_POINT('Ctrl Pts',(6.80909284730965,-1.02003530861282,5.55720583872655));
#11654=CARTESIAN_POINT('Ctrl Pts',(6.83891606812381,-0.968128023894585,
5.56116218872616));
#11655=CARTESIAN_POINT('Ctrl Pts',(6.93903973707845,-0.774161308408252,
5.57586192382845));
#11656=CARTESIAN_POINT('Ctrl Pts',(6.99467892489336,-0.625209072407786,
5.58704767703248));
#11657=CARTESIAN_POINT('Ctrl Pts',(7.04087087724725,-0.435229225625189,
5.60054735933996));
#11658=CARTESIAN_POINT('Ctrl Pts',(7.04862847847864,-0.398943341144046,
5.60308949825052));
#11659=CARTESIAN_POINT('Ctrl Pts',(7.06154546789643,-0.329039939068891,
5.60789423543807));
#11660=CARTESIAN_POINT('Ctrl Pts',(7.06686635442532,-0.295464519844523,
5.61016163083061));
#11661=CARTESIAN_POINT('Ctrl Pts',(7.07248325639656,-0.253032087660945,
5.61296330402136));
#11662=CARTESIAN_POINT('Ctrl Pts',(7.07358169342412,-0.244289130860153,
5.61353717323134));
#11663=CARTESIAN_POINT('Ctrl Pts',(7.07523088609569,-0.230420035832409,
5.61444182440976));
#11664=CARTESIAN_POINT('Ctrl Pts',(7.07581975063605,-0.225298670240397,
5.61477465306572));
#11665=CARTESIAN_POINT('Ctrl Pts',(7.07687646647887,-0.215783492915587,
5.6153906783008));
#11666=CARTESIAN_POINT('Ctrl Pts',(7.07734956885683,-0.211390448550495,
5.61567415237963));
#11667=CARTESIAN_POINT('Ctrl Pts',(7.07826738978968,-0.202593459585779,
5.61623996502225));
#11668=CARTESIAN_POINT('Ctrl Pts',(7.07871204673247,-0.198189613244848,
5.61652229810091));
#11669=CARTESIAN_POINT('Ctrl Pts',(7.07970451081397,-0.188021844236451,
5.61717211793837));
#11670=CARTESIAN_POINT('Ctrl Pts',(7.08024189179518,-0.182256911056624,
5.61753904057486));
#11671=CARTESIAN_POINT('Ctrl Pts',(7.08156992345348,-0.167305880330492,
5.61848690255623));
#11672=CARTESIAN_POINT('Ctrl Pts',(7.08232201005302,-0.158116380789593,
5.61906584813554));
#11673=CARTESIAN_POINT('Ctrl Pts',(7.08668811678998,-0.0997972750626993,
5.62271873905821));
#11674=CARTESIAN_POINT('Ctrl Pts',(7.0885451104228,-0.0505497564851107,
5.62570794647002));
#11675=CARTESIAN_POINT('Ctrl Pts',(7.0885767442888,-0.00128075752557987,
5.62864732406692));
#11676=CARTESIAN_POINT('Origin',(5.09382715545311,0.,-6.77268258743872));
#11677=CARTESIAN_POINT('',(7.08799995208786,0.00180011744721413,6.58540798502574));
#11678=CARTESIAN_POINT('',(7.08575281161347,-0.000877199754626239,6.42728338101755));
#11679=CARTESIAN_POINT('',(7.08857715545311,8.3550772080578E-14,-6.77268258743872));
#11680=CARTESIAN_POINT('Ctrl Pts',(7.08857636475715,0.00177608583532361,
6.58573943276249));
#11681=CARTESIAN_POINT('Ctrl Pts',(7.08868588516143,-0.121227957941686,
6.5785857802516));
#11682=CARTESIAN_POINT('Ctrl Pts',(7.07741849417107,-0.243966358813522,
6.57135126467452));
#11683=CARTESIAN_POINT('Ctrl Pts',(7.05234423754484,-0.378730559112279,
6.56287097820885));
#11684=CARTESIAN_POINT('Ctrl Pts',(7.04962091214582,-0.392551605440979,
6.56199514662556));
#11685=CARTESIAN_POINT('Ctrl Pts',(7.0448388108166,-0.415534888572078,6.56052792503132));
#11686=CARTESIAN_POINT('Ctrl Pts',(7.0428612841997,-0.424713648469547,6.55993908502373));
#11687=CARTESIAN_POINT('Ctrl Pts',(7.03885051728125,-0.44271163642731,6.55877863065602));
#11688=CARTESIAN_POINT('Ctrl Pts',(7.03682191011819,-0.45153167117863,6.55820717536531));
#11689=CARTESIAN_POINT('Ctrl Pts',(7.03287599826177,-0.468168693386053,
6.55712388466846));
#11690=CARTESIAN_POINT('Ctrl Pts',(7.03097126126369,-0.475988498272161,
6.55661246101819));
#11691=CARTESIAN_POINT('Ctrl Pts',(7.02655505291837,-0.493653388630137,
6.555451960513));
#11692=CARTESIAN_POINT('Ctrl Pts',(7.02401559601967,-0.503491182999488,
6.55480199617546));
#11693=CARTESIAN_POINT('Ctrl Pts',(7.01727740803145,-0.528794374278642,
6.55312060014303));
#11694=CARTESIAN_POINT('Ctrl Pts',(7.01296733249796,-0.54422910661841,6.55208561250086));
#11695=CARTESIAN_POINT('Ctrl Pts',(6.98028977524964,-0.656031838053373,
6.54451880485529));
#11696=CARTESIAN_POINT('Ctrl Pts',(6.94486879497236,-0.750172211367793,
6.53775761723513));
#11697=CARTESIAN_POINT('Ctrl Pts',(6.86897249569128,-0.913352557611503,
6.525367791711));
#11698=CARTESIAN_POINT('Ctrl Pts',(6.83114694481671,-0.983398666759867,
6.51980985448184));
#11699=CARTESIAN_POINT('Ctrl Pts',(6.74579068808271,-1.12109116298879,6.50852702427869));
#11700=CARTESIAN_POINT('Ctrl Pts',(6.69802966842602,-1.18842984258498,6.50281429888683));
#11701=CARTESIAN_POINT('Ctrl Pts',(6.63098314635375,-1.27152222488384,6.49566930776576));
#11702=CARTESIAN_POINT('Ctrl Pts',(6.6153886349375,-1.29014266664258,6.49406171368352));
#11703=CARTESIAN_POINT('Ctrl Pts',(6.59570284993209,-1.31279462133187,6.49210278028014));
#11704=CARTESIAN_POINT('Ctrl Pts',(6.59192992287261,-1.31709848516167,6.49173043477878));
#11705=CARTESIAN_POINT('Ctrl Pts',(6.58459340172728,-1.32539511129628,6.49101247095633));
#11706=CARTESIAN_POINT('Ctrl Pts',(6.58103216444069,-1.32938988447384,6.49066669086063));
#11707=CARTESIAN_POINT('Ctrl Pts',(6.57444766450176,-1.33671639097868,6.49003244467795));
#11708=CARTESIAN_POINT('Ctrl Pts',(6.57142921669363,-1.34005221953726,6.48974364492419));
#11709=CARTESIAN_POINT('Ctrl Pts',(6.56458100281913,-1.34756923025407,6.48909278569706));
#11710=CARTESIAN_POINT('Ctrl Pts',(6.56074468459922,-1.3517443080906,6.48873122574483));
#11711=CARTESIAN_POINT('Ctrl Pts',(6.55078883132367,-1.36248699708177,6.48780057671447));
#11712=CARTESIAN_POINT('Ctrl Pts',(6.54464259499581,-1.36902984249187,6.48723343593178));
#11713=CARTESIAN_POINT('Ctrl Pts',(6.50478443476463,-1.41089010897879,6.4836010639108));
#11714=CARTESIAN_POINT('Ctrl Pts',(6.46982666332094,-1.44500434442088,6.48062278840586));
#11715=CARTESIAN_POINT('Ctrl Pts',(6.42479727779275,-1.48582934945199,6.47698159327014));
#11716=CARTESIAN_POINT('Ctrl Pts',(6.41587342408448,-1.49377508158908,6.47626906459009));
#11717=CARTESIAN_POINT('Ctrl Pts',(6.39518572186291,-1.51186464509181,6.47463654951614));
#11718=CARTESIAN_POINT('Ctrl Pts',(6.38337364797385,-1.52195226014561,6.47371850038589));
#11719=CARTESIAN_POINT('Ctrl Pts',(6.27208399766122,-1.61476871193656,6.46518659431576));
#11720=CARTESIAN_POINT('Ctrl Pts',(6.16489715164525,-1.68777293012297,6.4578142807614));
#11721=CARTESIAN_POINT('Ctrl Pts',(6.00527869533838,-1.7751188799328,6.44705544387477));
#11722=CARTESIAN_POINT('Ctrl Pts',(5.95818713694719,-1.79851943863914,6.44390874471338));
#11723=CARTESIAN_POINT('Ctrl Pts',(5.88907060725803,-1.82952265885987,6.43928907392226));
#11724=CARTESIAN_POINT('Ctrl Pts',(5.8677492108992,-1.83864349276188,6.43786393305834));
#11725=CARTESIAN_POINT('Ctrl Pts',(5.8293914936377,-1.8542666961672,6.43529680069524));
#11726=CARTESIAN_POINT('Ctrl Pts',(5.81241568696985,-1.86091116506232,6.43415956034687));
#11727=CARTESIAN_POINT('Ctrl Pts',(5.78618742895198,-1.87076472328597,6.43239969182188));
#11728=CARTESIAN_POINT('Ctrl Pts',(5.77699814618326,-1.87414001348626,6.43178258936295));
#11729=CARTESIAN_POINT('Ctrl Pts',(5.7602360182227,-1.88015720423062,6.43065582822823));
#11730=CARTESIAN_POINT('Ctrl Pts',(5.75267133417024,-1.88282134843125,6.43014691797857));
#11731=CARTESIAN_POINT('Ctrl Pts',(5.73628836582741,-1.88848031093389,6.42904378788189));
#11732=CARTESIAN_POINT('Ctrl Pts',(5.72746479346409,-1.8914591273617,6.42844905501003));
#11733=CARTESIAN_POINT('Ctrl Pts',(5.70338303223282,-1.89940165380783,6.42682406630561));
#11734=CARTESIAN_POINT('Ctrl Pts',(5.68808555667229,-1.90424314022985,6.4257898474097));
#11735=CARTESIAN_POINT('Ctrl Pts',(5.60833989468399,-1.92842729848641,6.42038701336388));
#11736=CARTESIAN_POINT('Ctrl Pts',(5.54300826095254,-1.94468244149756,6.41591991230863));
#11737=CARTESIAN_POINT('Ctrl Pts',(5.32520046092084,-1.98731363355628,6.40089315838238));
#11738=CARTESIAN_POINT('Ctrl Pts',(5.17048024289048,-1.99926598901546,6.38995959937071));
#11739=CARTESIAN_POINT('Ctrl Pts',(4.95285321576843,-1.99076432141499,6.37495926291303));
#11740=CARTESIAN_POINT('Ctrl Pts',(4.88989105248304,-1.98530299760848,6.37067268747268));
#11741=CARTESIAN_POINT('Ctrl Pts',(4.81728023758988,-1.97551293202631,6.36586567029279));
#11742=CARTESIAN_POINT('Ctrl Pts',(4.80728242356727,-1.97408755359546,6.3652068378418));
#11743=CARTESIAN_POINT('Ctrl Pts',(4.79197267560127,-1.9717860962818,6.36420307923019));
#11744=CARTESIAN_POINT('Ctrl Pts',(4.78665291825287,-1.97096436450418,6.36385524756638));
#11745=CARTESIAN_POINT('Ctrl Pts',(4.7768950489558,-1.96941662045992,6.36321905527266));
#11746=CARTESIAN_POINT('Ctrl Pts',(4.7724560724592,-1.96869713589493,6.36293034602091));
#11747=CARTESIAN_POINT('Ctrl Pts',(4.76246277379203,-1.96704268680219,6.36228194801662));
#11748=CARTESIAN_POINT('Ctrl Pts',(4.7569099637623,-1.96609920729975,6.36192274171707));
#11749=CARTESIAN_POINT('Ctrl Pts',(4.74057326154863,-1.96325219006401,6.36086891396389));
#11750=CARTESIAN_POINT('Ctrl Pts',(4.72980075722238,-1.96128332208228,6.36017784164154));
#11751=CARTESIAN_POINT('Ctrl Pts',(4.62539686936041,-1.94131178911723,6.35351258287231));
#11752=CARTESIAN_POINT('Ctrl Pts',(4.53314055242254,-1.91670389972308,6.34787347598419));
#11753=CARTESIAN_POINT('Ctrl Pts',(4.32090649469527,-1.84344807320631,6.33476699576689));
#11754=CARTESIAN_POINT('Ctrl Pts',(4.20321101028993,-1.78955552884023,6.32737533679035));
#11755=CARTESIAN_POINT('Ctrl Pts',(4.03885400356676,-1.69404076667453,6.31601234957295));
#11756=CARTESIAN_POINT('Ctrl Pts',(3.98759223501989,-1.66101947040291,6.31230637370615));
#11757=CARTESIAN_POINT('Ctrl Pts',(3.92558874230334,-1.61693404851766,6.30757093813506));
#11758=CARTESIAN_POINT('Ctrl Pts',(3.91335230062993,-1.60802232711629,6.30662358057183));
#11759=CARTESIAN_POINT('Ctrl Pts',(3.89398806826986,-1.59357933436011,6.30510315128279));
#11760=CARTESIAN_POINT('Ctrl Pts',(3.88679416880441,-1.58813736649715,6.30453354190998));
#11761=CARTESIAN_POINT('Ctrl Pts',(3.87324778896266,-1.57774472973173,6.30345175350529));
#11762=CARTESIAN_POINT('Ctrl Pts',(3.86688788061656,-1.57280400395455,6.30293997164572));
#11763=CARTESIAN_POINT('Ctrl Pts',(3.85253358851301,-1.56151275388631,6.30177591697387));
#11764=CARTESIAN_POINT('Ctrl Pts',(3.84455774113881,-1.55513913330964,6.30112273512344));
#11765=CARTESIAN_POINT('Ctrl Pts',(3.8240625180685,-1.53850167475167,6.29942747639795));
#11766=CARTESIAN_POINT('Ctrl Pts',(3.8116187314131,-1.5281463180425,6.29838174484567));
#11767=CARTESIAN_POINT('Ctrl Pts',(3.69886274464726,-1.43196718413306,6.28875199764492));
#11768=CARTESIAN_POINT('Ctrl Pts',(3.60719451270669,-1.33655050243019,6.2797586371305));
#11769=CARTESIAN_POINT('Ctrl Pts',(3.46360698416528,-1.15389882219337,6.26361266981048));
#11770=CARTESIAN_POINT('Ctrl Pts',(3.40762260822076,-1.0704276645956,6.25656698823341));
#11771=CARTESIAN_POINT('Ctrl Pts',(3.33324589751594,-0.939114562229729,
6.24624510340067));
#11772=CARTESIAN_POINT('Ctrl Pts',(3.31001269947785,-0.894197667815707,
6.24283914849803));
#11773=CARTESIAN_POINT('Ctrl Pts',(3.28443493076994,-0.839773242290625,
6.23889768494268));
#11774=CARTESIAN_POINT('Ctrl Pts',(3.28042298910728,-0.83107440069057,6.23827321423748));
#11775=CARTESIAN_POINT('Ctrl Pts',(3.27430045197504,-0.817543839487553,
6.23731077499121));
#11776=CARTESIAN_POINT('Ctrl Pts',(3.27214614987967,-0.812732225052388,
6.23697025212102));
#11777=CARTESIAN_POINT('Ctrl Pts',(3.26818592381283,-0.803792236454992,
6.23634084164352));
#11778=CARTESIAN_POINT('Ctrl Pts',(3.26637492334548,-0.799666309176151,
6.23605165913068));
#11779=CARTESIAN_POINT('Ctrl Pts',(3.2622749027994,-0.790238731888157,6.23539381482357));
#11780=CARTESIAN_POINT('Ctrl Pts',(3.25999491422456,-0.784933258699513,
6.2350256998411));
#11781=CARTESIAN_POINT('Ctrl Pts',(3.25409385332693,-0.771035585981555,
6.23406669956338));
#11782=CARTESIAN_POINT('Ctrl Pts',(3.25050987935621,-0.762427652525928,
6.23347796515679));
#11783=CARTESIAN_POINT('Ctrl Pts',(3.22578059290626,-0.701839463813795,
6.22936867649569));
#11784=CARTESIAN_POINT('Ctrl Pts',(3.20677456883366,-0.649007220919063,
6.22596325599426));
#11785=CARTESIAN_POINT('Ctrl Pts',(3.1415365774367,-0.440420674228292,6.21294550242712));
#11786=CARTESIAN_POINT('Ctrl Pts',(3.11216592957644,-0.280058874966243,
6.20379410462717));
#11787=CARTESIAN_POINT('Ctrl Pts',(3.09858391842104,-0.0506729573932457,
6.1901136990173));
#11788=CARTESIAN_POINT('Ctrl Pts',(3.09801085941084,0.0167095540782358,
6.18603188695777));
#11789=CARTESIAN_POINT('Ctrl Pts',(3.10150236693872,0.0995614616089712,
6.1808734351888));
#11790=CARTESIAN_POINT('Ctrl Pts',(3.10234120444189,0.115127029242017,6.17989833378868));
#11791=CARTESIAN_POINT('Ctrl Pts',(3.10395977553171,0.13978029173327,6.17834379617816));
#11792=CARTESIAN_POINT('Ctrl Pts',(3.10461956890376,0.148875427108541,6.17776810307447));
#11793=CARTESIAN_POINT('Ctrl Pts',(3.10597825894061,0.16597874206437,6.17668126015351));
#11794=CARTESIAN_POINT('Ctrl Pts',(3.1066632474555,0.173987866953295,6.17617055511855));
#11795=CARTESIAN_POINT('Ctrl Pts',(3.10831381495862,0.192003647838789,6.1750177125317));
#11796=CARTESIAN_POINT('Ctrl Pts',(3.10930666443292,0.202007526326784,6.17437473427432));
#11797=CARTESIAN_POINT('Ctrl Pts',(3.11204063258,0.227585874381187,6.17272332476387));
#11798=CARTESIAN_POINT('Ctrl Pts',(3.11388972210581,0.243147875414463,6.17171154687424));
#11799=CARTESIAN_POINT('Ctrl Pts',(3.12750624921126,0.347259377547065,6.16489393125444));
#11800=CARTESIAN_POINT('Ctrl Pts',(3.14502533871208,0.434941982325944,6.15890863244901));
#11801=CARTESIAN_POINT('Ctrl Pts',(3.20246218588092,0.647153052977282,6.14384633564044));
#11802=CARTESIAN_POINT('Ctrl Pts',(3.24885096834211,0.769498702300583,6.13463940615336));
#11803=CARTESIAN_POINT('Ctrl Pts',(3.33491070833416,0.942987915869029,6.12130125916831));
#11804=CARTESIAN_POINT('Ctrl Pts',(3.36563797546309,0.998186919040296,6.11701632895041));
#11805=CARTESIAN_POINT('Ctrl Pts',(3.40425965165985,1.06042028283198,6.11221090894979));
#11806=CARTESIAN_POINT('Ctrl Pts',(3.40964942157835,1.06895972659542,6.11155212980415));
#11807=CARTESIAN_POINT('Ctrl Pts',(3.41801132295856,1.08198790668985,6.11054843515846));
#11808=CARTESIAN_POINT('Ctrl Pts',(3.4209370710774,1.0865060063837,6.11020061471496));
#11809=CARTESIAN_POINT('Ctrl Pts',(3.42634068867206,1.09477699475915,6.10956443314773));
#11810=CARTESIAN_POINT('Ctrl Pts',(3.42881295634264,1.09853334164469,6.1092757234837));
#11811=CARTESIAN_POINT('Ctrl Pts',(3.43441044857961,1.10697582645171,6.10862731238993));
#11812=CARTESIAN_POINT('Ctrl Pts',(3.43754282604389,1.111657100647,6.1082680935046));
#11813=CARTESIAN_POINT('Ctrl Pts',(3.44682379130446,1.12540100159068,6.10721419415414));
#11814=CARTESIAN_POINT('Ctrl Pts',(3.45302734729278,1.13442650629275,6.10652306354062));
#11815=CARTESIAN_POINT('Ctrl Pts',(3.51468984352989,1.22257470407039,6.09977767926405));
#11816=CARTESIAN_POINT('Ctrl Pts',(3.57576204010148,1.29763128039524,6.09406766015992));
#11817=CARTESIAN_POINT('Ctrl Pts',(3.7299196840154,1.46123369403699,6.08095066807389));
#11818=CARTESIAN_POINT('Ctrl Pts',(3.82657408992542,1.54580595301847,6.07361316082865));
#11819=CARTESIAN_POINT('Ctrl Pts',(3.97999409974984,1.65592560037629,6.06232292310008));
#11820=CARTESIAN_POINT('Ctrl Pts',(4.03090360349148,1.68905479899823,6.05863089631575));
#11821=CARTESIAN_POINT('Ctrl Pts',(4.09627672521156,1.72746904656913,6.05391118574962));
#11822=CARTESIAN_POINT('Ctrl Pts',(4.10939881743706,1.73498040198418,6.05296492662961));
#11823=CARTESIAN_POINT('Ctrl Pts',(4.13048032360395,1.74673173127524,6.051445847848));
#11824=CARTESIAN_POINT('Ctrl Pts',(4.13838546285367,1.7510682531575,6.0508764796131));
#11825=CARTESIAN_POINT('Ctrl Pts',(4.15340724356758,1.75917674571198,6.04979488531505));
#11826=CARTESIAN_POINT('Ctrl Pts',(4.16051787950756,1.76295950766066,6.04928305450948));
#11827=CARTESIAN_POINT('Ctrl Pts',(4.17669941756333,1.7714425327052,6.04811852512529));
#11828=CARTESIAN_POINT('Ctrl Pts',(4.18578385535764,1.77611635121095,6.04746491463593));
#11829=CARTESIAN_POINT('Ctrl Pts',(4.20937489597057,1.78802532030028,6.04576780656778));
#11830=CARTESIAN_POINT('Ctrl Pts',(4.22393428015434,1.79515367175058,6.04472064104634));
#11831=CARTESIAN_POINT('Ctrl Pts',(4.35612029080565,1.85788696661597,6.03521321890788));
#11832=CARTESIAN_POINT('Ctrl Pts',(4.47881571118974,1.90202653371074,6.02635622128806));
#11833=CARTESIAN_POINT('Ctrl Pts',(4.69502459895472,1.95668684785514,6.01086416603617));
#11834=CARTESIAN_POINT('Ctrl Pts',(4.78662006503553,1.97314244917739,6.00434350250644));
#11835=CARTESIAN_POINT('Ctrl Pts',(4.9378577813625,1.98952316765853,5.99388713425263));
#11836=CARTESIAN_POINT('Ctrl Pts',(4.99694638159507,1.99327480085813,5.98987992319688));
#11837=CARTESIAN_POINT('Ctrl Pts',(5.06607175913961,1.994581729572,5.98534512179595));
#11838=CARTESIAN_POINT('Ctrl Pts',(5.07602516429889,1.99469539953001,5.98469587396475));
#11839=CARTESIAN_POINT('Ctrl Pts',(5.09133122782593,1.99475561836228,5.98370362356004));
#11840=CARTESIAN_POINT('Ctrl Pts',(5.09668334776992,1.99475513545624,5.98335781538285));
#11841=CARTESIAN_POINT('Ctrl Pts',(5.10653421220646,1.99471459917883,5.9827235427726));
#11842=CARTESIAN_POINT('Ctrl Pts',(5.11103281022762,1.9946808686242,5.98243474446747));
#11843=CARTESIAN_POINT('Ctrl Pts',(5.12120040404407,1.99457023169572,5.98178391987169));
#11844=CARTESIAN_POINT('Ctrl Pts',(5.12686920255847,1.99448437670734,5.98142239286366));
#11845=CARTESIAN_POINT('Ctrl Pts',(5.14151083432827,1.99420018498417,5.98049188569986));
#11846=CARTESIAN_POINT('Ctrl Pts',(5.15048294642272,1.99396545593045,5.979924852849));
#11847=CARTESIAN_POINT('Ctrl Pts',(5.20821639025844,1.99206502771256,5.97629474655348));
#11848=CARTESIAN_POINT('Ctrl Pts',(5.25690860341288,1.988671231944,5.97331850450749));
#11849=CARTESIAN_POINT('Ctrl Pts',(5.31728010108539,1.98223064538762,5.96968121249203));
#11850=CARTESIAN_POINT('Ctrl Pts',(5.32911734907688,1.98086044023108,5.96897058481451));
#11851=CARTESIAN_POINT('Ctrl Pts',(5.38520518403725,1.97385819977351,5.96561267370825));
#11852=CARTESIAN_POINT('Ctrl Pts',(5.42927237319543,1.96684878227665,5.96300148241768));
#11853=CARTESIAN_POINT('Ctrl Pts',(5.57133238201177,1.93933858352787,5.95457363347082));
#11854=CARTESIAN_POINT('Ctrl Pts',(5.66802158756929,1.91294160767607,5.94881451204955));
#11855=CARTESIAN_POINT('Ctrl Pts',(5.81198766609175,1.86173359992015,5.9397804558131));
#11856=CARTESIAN_POINT('Ctrl Pts',(5.860932154065,1.84210635805048,5.9366252556888));
#11857=CARTESIAN_POINT('Ctrl Pts',(5.94059426360093,1.80643526784675,5.9313026189406));
#11858=CARTESIAN_POINT('Ctrl Pts',(5.9717747813277,1.79148839166356,5.92916998370932));
#11859=CARTESIAN_POINT('Ctrl Pts',(6.01364067741499,1.77006380354809,5.92623099915262));
#11860=CARTESIAN_POINT('Ctrl Pts',(6.02467794644827,1.76428443782323,5.92544889679229));
#11861=CARTESIAN_POINT('Ctrl Pts',(6.04310029870376,1.75441708226857,5.92413086376869));
#11862=CARTESIAN_POINT('Ctrl Pts',(6.05051497820353,1.75038487348025,5.92359690786228));
#11863=CARTESIAN_POINT('Ctrl Pts',(6.06507902678555,1.74234455283601,5.9225411301326));
#11864=CARTESIAN_POINT('Ctrl Pts',(6.07222972860703,1.73833919012566,5.92201941388445));
#11865=CARTESIAN_POINT('Ctrl Pts',(6.08790301402524,1.72943268253098,5.92086840419036));
#11866=CARTESIAN_POINT('Ctrl Pts',(6.09641441671951,1.72451239306663,5.92023843287208));
#11867=CARTESIAN_POINT('Ctrl Pts',(6.12614593860835,1.70703062995768,5.91802031641588));
#11868=CARTESIAN_POINT('Ctrl Pts',(6.14716847600234,1.69413919559536,5.91642030829377));
#11869=CARTESIAN_POINT('Ctrl Pts',(6.29419953114322,1.60018215093131,5.90499886780564));
#11870=CARTESIAN_POINT('Ctrl Pts',(6.41093889171826,1.50554890790296,5.89465691854766));
#11871=CARTESIAN_POINT('Ctrl Pts',(6.57572233686878,1.3380119975311,5.87827382636505));
#11872=CARTESIAN_POINT('Ctrl Pts',(6.63152697466188,1.27348745365528,5.87232928307388));
#11873=CARTESIAN_POINT('Ctrl Pts',(6.6986495627327,1.18500633203405,5.8647969850376));
#11874=CARTESIAN_POINT('Ctrl Pts',(6.71386269417006,1.16412196502821,5.86306099067059));
#11875=CARTESIAN_POINT('Ctrl Pts',(6.73859882267876,1.12874009896752,5.86019640978647));
#11876=CARTESIAN_POINT('Ctrl Pts',(6.74834591644032,1.11440377182698,5.85905604912421));
#11877=CARTESIAN_POINT('Ctrl Pts',(6.7615930255724,1.09436250448009,5.8574918155903));
#11878=CARTESIAN_POINT('Ctrl Pts',(6.76525276657489,1.08876476721394,5.85705809418005));
#11879=CARTESIAN_POINT('Ctrl Pts',(6.77140541029616,1.07924988643152,5.85632638830238));
#11880=CARTESIAN_POINT('Ctrl Pts',(6.77391289635154,1.07534228193641,5.85602745493481));
#11881=CARTESIAN_POINT('Ctrl Pts',(6.77869388944691,1.06783415500849,5.85545612710434));
#11882=CARTESIAN_POINT('Ctrl Pts',(6.78096953232191,1.06423507502839,5.85518358597631));
#11883=CARTESIAN_POINT('Ctrl Pts',(6.78638888631956,1.05560293832246,5.85453302162247));
#11884=CARTESIAN_POINT('Ctrl Pts',(6.78952171943477,1.05056305094438,5.85415570360883));
#11885=CARTESIAN_POINT('Ctrl Pts',(6.80072717097473,1.03235577319717,5.85280134377055));
#11886=CARTESIAN_POINT('Ctrl Pts',(6.80866953204444,1.01910831764367,5.85183233459209));
#11887=CARTESIAN_POINT('Ctrl Pts',(6.88317649851434,0.891496609000298,5.84264060976615));
#11888=CARTESIAN_POINT('Ctrl Pts',(6.93836916982898,0.77085149699917,5.83502325095135));
#11889=CARTESIAN_POINT('Ctrl Pts',(7.01224752832938,0.554876165668998,5.82177037532876));
#11890=CARTESIAN_POINT('Ctrl Pts',(7.03670057593788,0.462023006619127,5.81618658301961));
#11891=CARTESIAN_POINT('Ctrl Pts',(7.06068878825422,0.334146261795293,5.80835987917839));
#11892=CARTESIAN_POINT('Ctrl Pts',(7.06613090174208,0.300360025497406,5.80628023153093));
#11893=CARTESIAN_POINT('Ctrl Pts',(7.07404047656506,0.241676884494521,5.80263652542301));
#11894=CARTESIAN_POINT('Ctrl Pts',(7.07691360873699,0.216842214571727,5.80108484087109));
#11895=CARTESIAN_POINT('Ctrl Pts',(7.08037599338972,0.18103004777908,5.79883057628999));
#11896=CARTESIAN_POINT('Ctrl Pts',(7.08134250808545,0.170090796509527,5.79813975591724));
#11897=CARTESIAN_POINT('Ctrl Pts',(7.08286965557643,0.151010206342768,5.7969306891822));
#11898=CARTESIAN_POINT('Ctrl Pts',(7.08347075476179,0.142872300440119,5.79641371751136));
#11899=CARTESIAN_POINT('Ctrl Pts',(7.08453639554149,0.127131066677307,5.79541112337759));
#11900=CARTESIAN_POINT('Ctrl Pts',(7.08500735035069,0.119528304160802,5.79492571048008));
#11901=CARTESIAN_POINT('Ctrl Pts',(7.08602425909707,0.10143299692379,5.79376750146164));
#11902=CARTESIAN_POINT('Ctrl Pts',(7.08653087782553,0.0909385534460679,
5.79309349118482));
#11903=CARTESIAN_POINT('Ctrl Pts',(7.08804761810333,0.0533573994625538,
5.7906713111105));
#11904=CARTESIAN_POINT('Ctrl Pts',(7.08858849020073,0.0262557374264677,
5.78890867927665));
#11905=CARTESIAN_POINT('Ctrl Pts',(7.08857697543024,-0.000847467537911379,
5.78712926964944));
#11906=CARTESIAN_POINT('Ctrl Pts',(7.09089102510648,-0.00118553947171295,
5.62731851852589));
#11907=CARTESIAN_POINT('Ctrl Pts',(7.0866941324795,0.587071456722144,5.66499078781088));
#11908=CARTESIAN_POINT('Ctrl Pts',(6.50103913263564,1.84272192090518,5.74493881493197));
#11909=CARTESIAN_POINT('Ctrl Pts',(4.36834791099822,2.24206777668213,5.8671625998891));
#11910=CARTESIAN_POINT('Ctrl Pts',(2.81757555877128,0.60980875524591,5.99398987339733));
#11911=CARTESIAN_POINT('Ctrl Pts',(3.34465352606379,-1.57910723626363,6.12081714690552));
#11912=CARTESIAN_POINT('Ctrl Pts',(5.46844469940953,-2.32655318983495,6.24764442041377));
#11913=CARTESIAN_POINT('Ctrl Pts',(6.90380566236945,-1.21784869222614,6.34981092595642));
#11914=CARTESIAN_POINT('Ctrl Pts',(7.08678277106929,-0.277777213867225,
6.40970167366304));
#11915=CARTESIAN_POINT('Ctrl Pts',(7.08569500892407,-0.000879430567275395,
6.42731666353357));
#11916=CARTESIAN_POINT('Origin',(5.09382715545311,0.,-6.77268258743872));
#11917=CARTESIAN_POINT('',(7.08880671528828,-0.000547014378622251,7.38540769406316));
#11918=CARTESIAN_POINT('',(7.08857715545311,1.12756902441053E-10,7.22671373997843));
#11919=CARTESIAN_POINT('',(7.08857715545311,8.3550772080578E-14,-6.77268258743872));
#11920=CARTESIAN_POINT('Ctrl Pts',(7.08799995208786,0.00180011744721413,
6.58540798502575));
#11921=CARTESIAN_POINT('Ctrl Pts',(7.08953512162655,0.175492382420182,6.59648979094105));
#11922=CARTESIAN_POINT('Ctrl Pts',(6.98930587567619,1.01005559039421,6.64984735469243));
#11923=CARTESIAN_POINT('Ctrl Pts',(5.82074642522589,2.24160127242978,6.74548067627989));
#11924=CARTESIAN_POINT('Ctrl Pts',(3.6074629237785,1.8286359014643,6.8723079497881));
#11925=CARTESIAN_POINT('Ctrl Pts',(2.75099006585116,-0.253578904704738,
6.99913522329632));
#11926=CARTESIAN_POINT('Ctrl Pts',(4.03314933554441,-2.10431709865207,7.12596249680453));
#11927=CARTESIAN_POINT('Ctrl Pts',(6.28353626083478,-2.03415341945925,7.25278977031275));
#11928=CARTESIAN_POINT('Ctrl Pts',(7.07750672725613,-0.720147580231949,
7.33927148796819));
#11929=CARTESIAN_POINT('Ctrl Pts',(7.09175163085572,-0.0306588661273706,
7.38347744778755));
#11930=CARTESIAN_POINT('Ctrl Pts',(7.09164127533163,-0.000548482464498706,
7.38540764977084));
#11931=CARTESIAN_POINT('Ctrl Pts',(7.08857700753049,-0.000768203926909726,
6.42565722232425));
#11932=CARTESIAN_POINT('Ctrl Pts',(7.088589330516,0.0312301661132295,6.42760907927267));
#11933=CARTESIAN_POINT('Ctrl Pts',(7.08783171184399,0.063223026411317,6.42958181074859));
#11934=CARTESIAN_POINT('Ctrl Pts',(7.08582640600588,0.105200426417907,6.43220396661624));
#11935=CARTESIAN_POINT('Ctrl Pts',(7.08527231960211,0.11521413248421,6.43283199971842));
#11936=CARTESIAN_POINT('Ctrl Pts',(7.08415202477829,0.133024748424536,6.43395371348444));
#11937=CARTESIAN_POINT('Ctrl Pts',(7.08361544750926,0.14082336152514,6.43444646876064));
#11938=CARTESIAN_POINT('Ctrl Pts',(7.08245151325584,0.156402205302053,6.43543410627943));
#11939=CARTESIAN_POINT('Ctrl Pts',(7.08182430166488,0.164182307533372,6.43592897552786));
#11940=CARTESIAN_POINT('Ctrl Pts',(7.0803849649628,0.180816726927487,6.43699064321805));
#11941=CARTESIAN_POINT('Ctrl Pts',(7.07955927010025,0.18966967052163,6.43755785561866));
#11942=CARTESIAN_POINT('Ctrl Pts',(7.07722641192135,0.212994497171477,6.43905819699522));
#11943=CARTESIAN_POINT('Ctrl Pts',(7.07562006807252,0.227455708516326,6.43999440567719));
#11944=CARTESIAN_POINT('Ctrl Pts',(7.06803439219472,0.289547461014513,6.44404084680819));
#11945=CARTESIAN_POINT('Ctrl Pts',(7.06049540060659,0.336967817662538,6.44719931815086));
#11946=CARTESIAN_POINT('Ctrl Pts',(7.01788942838625,0.554112428174759,6.46198743990834));
#11947=CARTESIAN_POINT('Ctrl Pts',(6.96250985046776,0.719071621946716,6.47423393457015));
#11948=CARTESIAN_POINT('Ctrl Pts',(6.8572288289548,0.934831185141043,6.49079698832607));
#11949=CARTESIAN_POINT('Ctrl Pts',(6.82491453567728,0.993394802674202,6.49534261866924));
#11950=CARTESIAN_POINT('Ctrl Pts',(6.78433695249872,1.05891860529282,6.50040028558089));
#11951=CARTESIAN_POINT('Ctrl Pts',(6.77888995813123,1.06756514938461,6.50106708023694));
#11952=CARTESIAN_POINT('Ctrl Pts',(6.77045892410519,1.08072324061857,6.50208038869031));
#11953=CARTESIAN_POINT('Ctrl Pts',(6.7675226794871,1.0852649929698,6.50242989212538));
#11954=CARTESIAN_POINT('Ctrl Pts',(6.76211176379092,1.09356035053195,6.50306769244988));
#11955=CARTESIAN_POINT('Ctrl Pts',(6.75964287557799,1.09731753020336,6.50335635008455));
#11956=CARTESIAN_POINT('Ctrl Pts',(6.75406853295796,1.10573845155242,6.50400284181164));
#11957=CARTESIAN_POINT('Ctrl Pts',(6.7509561245584,1.11039746776133,6.50436020684622));
#11958=CARTESIAN_POINT('Ctrl Pts',(6.74177939564698,1.12400974665107,6.50540358419423));
#11959=CARTESIAN_POINT('Ctrl Pts',(6.73566174026383,1.13292705190093,6.50608615174947));
#11960=CARTESIAN_POINT('Ctrl Pts',(6.68512509943597,1.20532185563022,6.5116237084101));
#11961=CARTESIAN_POINT('Ctrl Pts',(6.63710946745687,1.26621977734296,6.51625863451744));
#11962=CARTESIAN_POINT('Ctrl Pts',(6.5108401767444,1.40847696402522,6.5274421148469));
#11963=CARTESIAN_POINT('Ctrl Pts',(6.42900242764555,1.48628434538825,6.53389097054297));
#11964=CARTESIAN_POINT('Ctrl Pts',(6.29320798742841,1.59507614532385,6.5441168470746));
#11965=CARTESIAN_POINT('Ctrl Pts',(6.24364977083468,1.6311619721759,6.54776175521778));
#11966=CARTESIAN_POINT('Ctrl Pts',(6.17103591330139,1.67908038347948,6.55304922787306));
#11967=CARTESIAN_POINT('Ctrl Pts',(6.14928828952595,1.69283529873874,6.55462620792526));
#11968=CARTESIAN_POINT('Ctrl Pts',(6.11524711434376,1.71345463574606,6.55708845322561));
#11969=CARTESIAN_POINT('Ctrl Pts',(6.10313629898589,1.72061633097482,6.55796325596448));
#11970=CARTESIAN_POINT('Ctrl Pts',(6.08282489038284,1.73233919086986,6.55942901299348));
#11971=CARTESIAN_POINT('Ctrl Pts',(6.07466593590645,1.73697175392102,6.56001742514646));
#11972=CARTESIAN_POINT('Ctrl Pts',(6.05871510179123,1.74588023820364,6.56116722657081));
#11973=CARTESIAN_POINT('Ctrl Pts',(6.05092671750115,1.75016198660145,6.56172839267283));
#11974=CARTESIAN_POINT('Ctrl Pts',(6.03610105416949,1.75818399829576,6.56279625593172));
#11975=CARTESIAN_POINT('Ctrl Pts',(6.02906944931659,1.76193442580175,6.56330258036936));
#11976=CARTESIAN_POINT('Ctrl Pts',(6.01312146941879,1.77031819018743,6.56445070783866));
#11977=CARTESIAN_POINT('Ctrl Pts',(6.00419223193426,1.77492646372661,6.56509337539839));
#11978=CARTESIAN_POINT('Ctrl Pts',(5.98126269392423,1.78654158256391,6.5667434545896));
#11979=CARTESIAN_POINT('Ctrl Pts',(5.96721423557539,1.79345132254698,6.56775420370496));
#11980=CARTESIAN_POINT('Ctrl Pts',(5.87317938406065,1.83833551935137,6.57451969383595));
#11981=CARTESIAN_POINT('Ctrl Pts',(5.79083298736072,1.87110833829854,6.58045060811876));
#11982=CARTESIAN_POINT('Ctrl Pts',(5.58170905287068,1.93861280681789,6.59550082587848));
#11983=CARTESIAN_POINT('Ctrl Pts',(5.45316275616061,1.9665001945574,6.60475674092297));
#11984=CARTESIAN_POINT('Ctrl Pts',(5.25997853114852,1.98882437221507,6.61815134042512));
#11985=CARTESIAN_POINT('Ctrl Pts',(5.19682558758413,1.99309349605632,6.62244482279055));
#11986=CARTESIAN_POINT('Ctrl Pts',(5.12347059201432,1.99455530814901,6.62725854454443));
#11987=CARTESIAN_POINT('Ctrl Pts',(5.11336907237617,1.99467985760589,6.62791760047651));
#11988=CARTESIAN_POINT('Ctrl Pts',(5.09788338736835,1.9947531404102,6.62892162729713));
#11989=CARTESIAN_POINT('Ctrl Pts',(5.09249982487867,1.99475682328346,6.62926950603586));
#11990=CARTESIAN_POINT('Ctrl Pts',(5.08261934727396,1.9947235823004,6.62990574339872));
#11991=CARTESIAN_POINT('Ctrl Pts',(5.07812257863614,1.99469324754727,6.63019445098651));
#11992=CARTESIAN_POINT('Ctrl Pts',(5.0679946493747,1.99459067412349,6.63084279431774));
#11993=CARTESIAN_POINT('Ctrl Pts',(5.06236367733891,1.99450979618571,6.63120194799081));
#11994=CARTESIAN_POINT('Ctrl Pts',(5.04578838650649,1.99420151089887,6.6322554762103));
#11995=CARTESIAN_POINT('Ctrl Pts',(5.03484530242939,1.99390785723189,6.63294630463898));
#11996=CARTESIAN_POINT('Ctrl Pts',(4.93508607267919,1.99040883252325,6.63920551728749));
#11997=CARTESIAN_POINT('Ctrl Pts',(4.8465625446466,1.9813607383178,6.64448338156183));
#11998=CARTESIAN_POINT('Ctrl Pts',(4.64395070552254,1.94685436265891,6.65650785784992));
#11999=CARTESIAN_POINT('Ctrl Pts',(4.53091477043828,1.9172272535737,6.66318493386606));
#12000=CARTESIAN_POINT('Ctrl Pts',(4.3726003549376,1.86051475586336,6.67313652737869));
#12001=CARTESIAN_POINT('Ctrl Pts',(4.32478052515999,1.84126314390431,6.67622371435591));
#12002=CARTESIAN_POINT('Ctrl Pts',(4.25688872568664,1.8108243706271,6.68076313422834));
#12003=CARTESIAN_POINT('Ctrl Pts',(4.23617861310828,1.80110792326424,6.68216946389145));
#12004=CARTESIAN_POINT('Ctrl Pts',(4.19926988472657,1.78301073778736,6.6847179516348));
#12005=CARTESIAN_POINT('Ctrl Pts',(4.18301025760501,1.77475985586078,6.68585568532457));
#12006=CARTESIAN_POINT('Ctrl Pts',(4.15829028429042,1.76178663089958,6.68760966345852));
#12007=CARTESIAN_POINT('Ctrl Pts',(4.14974716043247,1.75722347122054,6.68822033007702));
#12008=CARTESIAN_POINT('Ctrl Pts',(4.13426132758719,1.74880645955735,6.68933564428653));
#12009=CARTESIAN_POINT('Ctrl Pts',(4.12730771570866,1.74497300283502,6.68983956132312));
#12010=CARTESIAN_POINT('Ctrl Pts',(4.11219751411522,1.736524872572,6.69094146254863));
#12011=CARTESIAN_POINT('Ctrl Pts',(4.10405021751505,1.73189404814822,6.69154001530179));
#12012=CARTESIAN_POINT('Ctrl Pts',(4.08181994219555,1.71905053370222,6.69318550902097));
#12013=CARTESIAN_POINT('Ctrl Pts',(4.06780478633334,1.71072248160849,6.69423658091199));
#12014=CARTESIAN_POINT('Ctrl Pts',(3.99314426638532,1.66511039494194,6.69991095572775));
#12015=CARTESIAN_POINT('Ctrl Pts',(3.93443216758976,1.62477588077883,6.7046450834709));
#12016=CARTESIAN_POINT('Ctrl Pts',(3.76155603451837,1.4918638012132,6.71944374798924));
#12017=CARTESIAN_POINT('Ctrl Pts',(3.65535616137471,1.38974742759567,6.72981331261377));
#12018=CARTESIAN_POINT('Ctrl Pts',(3.51886054351958,1.2259330602287,6.74452104307906));
#12019=CARTESIAN_POINT('Ctrl Pts',(3.47894450916726,1.17285448677464,6.74903328608398));
#12020=CARTESIAN_POINT('Ctrl Pts',(3.43602710302209,1.10942808261533,6.75405874102827));
#12021=CARTESIAN_POINT('Ctrl Pts',(3.43037345108991,1.10093299902366,6.75472455620501));
#12022=CARTESIAN_POINT('Ctrl Pts',(3.42182511642405,1.08787221595719,6.75573669039174));
#12023=CARTESIAN_POINT('Ctrl Pts',(3.41888348863311,1.08333766269633,6.75608598863347));
#12024=CARTESIAN_POINT('Ctrl Pts',(3.41352882446706,1.07500943934847,6.7567235905653));
#12025=CARTESIAN_POINT('Ctrl Pts',(3.41111018312187,1.07121957023783,6.75701225351547));
#12026=CARTESIAN_POINT('Ctrl Pts',(3.40570420658077,1.0626852328549,6.75765897463491));
#12027=CARTESIAN_POINT('Ctrl Pts',(3.40272405249047,1.05793633628343,6.75801656212584));
#12028=CARTESIAN_POINT('Ctrl Pts',(3.3940459127365,1.04397728923754,6.75906119949848));
#12029=CARTESIAN_POINT('Ctrl Pts',(3.38840275810082,1.03473305291156,6.75974479211849));
#12030=CARTESIAN_POINT('Ctrl Pts',(3.34245167747488,0.958061866202165,6.76535101036473));
#12031=CARTESIAN_POINT('Ctrl Pts',(3.30607881586456,0.888345361085753,6.77004731096961));
#12032=CARTESIAN_POINT('Ctrl Pts',(3.23491930187805,0.729766656506672,6.7802611830524));
#12033=CARTESIAN_POINT('Ctrl Pts',(3.20220093285155,0.640194297382251,6.78573181649191));
#12034=CARTESIAN_POINT('Ctrl Pts',(3.1490691440313,0.454462518042895,6.79701942217045));
#12035=CARTESIAN_POINT('Ctrl Pts',(3.12910648613203,0.358454003972758,6.8028280116879));
#12036=CARTESIAN_POINT('Ctrl Pts',(3.1131899422585,0.238030016388062,6.81031398040511));
#12037=CARTESIAN_POINT('Ctrl Pts',(3.11051816884492,0.214633292099132,6.81177712254252));
#12038=CARTESIAN_POINT('Ctrl Pts',(3.10723347154922,0.18052169912609,6.81392534033777));
#12039=CARTESIAN_POINT('Ctrl Pts',(3.10629176475914,0.169839960976826,6.81460016488108));
#12040=CARTESIAN_POINT('Ctrl Pts',(3.10478841379868,0.151057524783607,6.81579071296601));
#12041=CARTESIAN_POINT('Ctrl Pts',(3.10419001777288,0.142959955203459,6.81630527769629));
#12042=CARTESIAN_POINT('Ctrl Pts',(3.10312109258738,0.127185263389626,6.81731029282065));
#12043=CARTESIAN_POINT('Ctrl Pts',(3.10264549443576,0.119508619201005,6.81780057551906));
#12044=CARTESIAN_POINT('Ctrl Pts',(3.10148772739044,0.0988895192001237,
6.81912076480896));
#12045=CARTESIAN_POINT('Ctrl Pts',(3.1008872873851,0.0859430206096428,6.81995320150754));
#12046=CARTESIAN_POINT('Ctrl Pts',(3.09912397962355,0.0377869164479501,
6.82306309524128));
#12047=CARTESIAN_POINT('Ctrl Pts',(3.09876780363548,0.00255601406838469,
6.82536533871372));
#12048=CARTESIAN_POINT('Ctrl Pts',(3.10264189845513,-0.233997828987448,
6.84101425760592));
#12049=CARTESIAN_POINT('Ctrl Pts',(3.13640900401216,-0.433655522898617,
6.85531829962411));
#12050=CARTESIAN_POINT('Ctrl Pts',(3.21687633452901,-0.677625253041591,
6.87294230081636));
#12051=CARTESIAN_POINT('Ctrl Pts',(3.2364987396808,-0.72969359935644,6.87670082602437));
#12052=CARTESIAN_POINT('Ctrl Pts',(3.26211397568363,-0.789905453433661,
6.88099151569122));
#12053=CARTESIAN_POINT('Ctrl Pts',(3.2660208929067,-0.798904296097861,6.88163125799971));
#12054=CARTESIAN_POINT('Ctrl Pts',(3.27214929079101,-0.812739587393907,
6.88261208196265));
#12055=CARTESIAN_POINT('Ctrl Pts',(3.27432393918432,-0.817596432905007,
6.88295587163263));
#12056=CARTESIAN_POINT('Ctrl Pts',(3.27837384508788,-0.826545280148521,
6.88358826024913));
#12057=CARTESIAN_POINT('Ctrl Pts',(3.2802435086024,-0.830639620305563,6.88387717826503));
#12058=CARTESIAN_POINT('Ctrl Pts',(3.28451566175652,-0.839911937439372,
6.88453056215311));
#12059=CARTESIAN_POINT('Ctrl Pts',(3.28692652539578,-0.845085947648634,
6.88489451123191));
#12060=CARTESIAN_POINT('Ctrl Pts',(3.29323957955067,-0.8584840147509,6.88583546459706));
#12061=CARTESIAN_POINT('Ctrl Pts',(3.29717596348398,-0.86669194287413,6.88641044802648));
#12062=CARTESIAN_POINT('Ctrl Pts',(3.32372071894968,-0.921083489930184,
6.89021281952478));
#12063=CARTESIAN_POINT('Ctrl Pts',(3.34805349585162,-0.966409285495142,
6.89334365658083));
#12064=CARTESIAN_POINT('Ctrl Pts',(3.40261655431234,-1.05924436249546,6.89978093537112));
#12065=CARTESIAN_POINT('Ctrl Pts',(3.43316006067346,-1.10651584807978,6.90307357280106));
#12066=CARTESIAN_POINT('Ctrl Pts',(3.46775923923249,-1.15539771051408,6.90655958852362));
#12067=CARTESIAN_POINT('Ctrl Pts',(3.46986435755691,-1.15835468174972,6.90677078977692));
#12068=CARTESIAN_POINT('Ctrl Pts',(3.53986360352071,-1.25611380871563,6.91376450064198));
#12069=CARTESIAN_POINT('Ctrl Pts',(3.61592801456458,-1.3447814324059,6.92047591178594));
#12070=CARTESIAN_POINT('Ctrl Pts',(3.72732839054369,-1.4537005618482,6.9297986652576));
#12071=CARTESIAN_POINT('Ctrl Pts',(3.75615763737576,-1.48027165674936,6.93217054853875));
#12072=CARTESIAN_POINT('Ctrl Pts',(3.80669213948574,-1.5241655065836,6.93627819135072));
#12073=CARTESIAN_POINT('Ctrl Pts',(3.8280109015467,-1.54191638398348,6.93799671527219));
#12074=CARTESIAN_POINT('Ctrl Pts',(3.85863696109675,-1.56635363132014,6.94044947902455));
#12075=CARTESIAN_POINT('Ctrl Pts',(3.86764293220926,-1.57341372707795,6.94116883620664));
#12076=CARTESIAN_POINT('Ctrl Pts',(3.8832376895765,-1.585423795647,6.9424114818964));
#12077=CARTESIAN_POINT('Ctrl Pts',(3.88979738686526,-1.59041119832056,6.94293328459356));
#12078=CARTESIAN_POINT('Ctrl Pts',(3.90239520124193,-1.59986683277711,6.94393378909102));
#12079=CARTESIAN_POINT('Ctrl Pts',(3.90842803551236,-1.60434189250607,6.94441221306948));
#12080=CARTESIAN_POINT('Ctrl Pts',(3.92415907502342,-1.61587375637479,6.94565802220415));
#12081=CARTESIAN_POINT('Ctrl Pts',(3.93389579415364,-1.62287727250695,6.94642743959259));
#12082=CARTESIAN_POINT('Ctrl Pts',(3.9620854506607,-1.6427705008603,6.9486505903565));
#12083=CARTESIAN_POINT('Ctrl Pts',(3.98069369025704,-1.65543590183602,6.95011270753178));
#12084=CARTESIAN_POINT('Ctrl Pts',(4.11851657998183,-1.74586834887584,6.96090644211711));
#12085=CARTESIAN_POINT('Ctrl Pts',(4.2455163743465,-1.81097820009745,6.97070492623463));
#12086=CARTESIAN_POINT('Ctrl Pts',(4.48669904769094,-1.90365425472071,6.98871272511691));
#12087=CARTESIAN_POINT('Ctrl Pts',(4.59849973863503,-1.93575808473208,6.99683561542773));
#12088=CARTESIAN_POINT('Ctrl Pts',(4.73094334588759,-1.96155480881843,7.00580634979991));
#12089=CARTESIAN_POINT('Ctrl Pts',(4.74947153372208,-1.9648921585735,7.0070464839901));
#12090=CARTESIAN_POINT('Ctrl Pts',(4.77485914782911,-1.9690948880131,7.00872301792543));
#12091=CARTESIAN_POINT('Ctrl Pts',(4.78167925345538,-1.97018754400765,7.0091711682355));
#12092=CARTESIAN_POINT('Ctrl Pts',(4.79313652147584,-1.9719621372078,7.00992012792961));
#12093=CARTESIAN_POINT('Ctrl Pts',(4.79777061262188,-1.9726631878765,7.0102219888622));
#12094=CARTESIAN_POINT('Ctrl Pts',(4.80657662619298,-1.97396364179228,7.01079352182552));
#12095=CARTESIAN_POINT('Ctrl Pts',(4.8107480330261,-1.9745661642311,7.01106337251019));
#12096=CARTESIAN_POINT('Ctrl Pts',(4.82172835384005,-1.97611666245945,7.01177144401466));
#12097=CARTESIAN_POINT('Ctrl Pts',(4.82854038533407,-1.97704267895438,7.01220844554638));
#12098=CARTESIAN_POINT('Ctrl Pts',(4.85246390663301,-1.98016892756954,7.01373562138544));
#12099=CARTESIAN_POINT('Ctrl Pts',(4.8695995845821,-1.9821824444351,7.01481594844347));
#12100=CARTESIAN_POINT('Ctrl Pts',(5.08690251218825,-2.00486234532082,7.02836913206812));
#12101=CARTESIAN_POINT('Ctrl Pts',(5.28908143376296,-1.99535046974311,7.03950502141961));
#12102=CARTESIAN_POINT('Ctrl Pts',(5.55844892346884,-1.94127494580665,7.05580352201697));
#12103=CARTESIAN_POINT('Ctrl Pts',(5.62959721699718,-1.92285476564722,7.06024139690932));
#12104=CARTESIAN_POINT('Ctrl Pts',(5.71477494156892,-1.89570734080917,7.06579975861128));
#12105=CARTESIAN_POINT('Ctrl Pts',(5.72992787543424,-1.89067668465797,7.06679813131708));
#12106=CARTESIAN_POINT('Ctrl Pts',(5.75371584306949,-1.88246092927145,7.0683812700384));
#12107=CARTESIAN_POINT('Ctrl Pts',(5.76239222626734,-1.87939697025274,7.06896205030836));
#12108=CARTESIAN_POINT('Ctrl Pts',(5.77859904737152,-1.87354729920393,7.07005332889127));
#12109=CARTESIAN_POINT('Ctrl Pts',(5.78613449217919,-1.87077592852671,7.07056334349911));
#12110=CARTESIAN_POINT('Ctrl Pts',(5.80295594089279,-1.8644738191269,7.0717078239135));
#12111=CARTESIAN_POINT('Ctrl Pts',(5.81223266141324,-1.86091906854542,7.07234307869535));
#12112=CARTESIAN_POINT('Ctrl Pts',(5.83571199155859,-1.8517202856674,7.07396150768721));
#12113=CARTESIAN_POINT('Ctrl Pts',(5.84987680044445,-1.84598213404487,7.07494780498331));
#12114=CARTESIAN_POINT('Ctrl Pts',(5.93720829072673,-1.80943046351508,7.08109164187705));
#12115=CARTESIAN_POINT('Ctrl Pts',(6.0085381787257,-1.7744382999037,7.0863895355258));
#12116=CARTESIAN_POINT('Ctrl Pts',(6.19895612433764,-1.66648802149252,7.10131223445727));
#12117=CARTESIAN_POINT('Ctrl Pts',(6.31276882181629,-1.58513988391596,7.11115899329005));
#12118=CARTESIAN_POINT('Ctrl Pts',(6.46561003801874,-1.44963223084906,7.1252380157083));
#12119=CARTESIAN_POINT('Ctrl Pts',(6.51195451302183,-1.40432847990216,7.12963760838606));
#12120=CARTESIAN_POINT('Ctrl Pts',(6.56292253160599,-1.34940335437977,7.13455417946827));
#12121=CARTESIAN_POINT('Ctrl Pts',(6.56977164816174,-1.34190852963138,7.13521658941542));
#12122=CARTESIAN_POINT('Ctrl Pts',(6.58017177448727,-1.33035195834597,7.13622464005901));
#12123=CARTESIAN_POINT('Ctrl Pts',(6.58376390796898,-1.32632768755214,7.13657322393231));
#12124=CARTESIAN_POINT('Ctrl Pts',(6.59032031342916,-1.31892229042792,7.13721013740142));
#12125=CARTESIAN_POINT('Ctrl Pts',(6.59328947514359,-1.31554571668826,7.13749882108049));
#12126=CARTESIAN_POINT('Ctrl Pts',(6.59994345535824,-1.30792691920996,7.13814635079389));
#12127=CARTESIAN_POINT('Ctrl Pts',(6.60362177615879,-1.30367915530447,7.13850472045696));
#12128=CARTESIAN_POINT('Ctrl Pts',(6.61437491097847,-1.29115476927748,7.13955379369074));
#12129=CARTESIAN_POINT('Ctrl Pts',(6.6214000992721,-1.28283554242252,7.1402409958054));
#12130=CARTESIAN_POINT('Ctrl Pts',(6.69210058800496,-1.19770764831555,7.14718058172315));
#12131=CARTESIAN_POINT('Ctrl Pts',(6.7500054196207,-1.11627086405036,7.1530652823694));
#12132=CARTESIAN_POINT('Ctrl Pts',(6.86656150814653,-0.923175627275076,
7.1662148909185));
#12133=CARTESIAN_POINT('Ctrl Pts',(6.92121670711533,-0.809621173809221,
7.17342389070417));
#12134=CARTESIAN_POINT('Ctrl Pts',(6.98567243080275,-0.635268491632854,
7.18454110637366));
#12135=CARTESIAN_POINT('Ctrl Pts',(7.00396303706933,-0.57794849676137,7.18819944472896));
#12136=CARTESIAN_POINT('Ctrl Pts',(7.02356493399509,-0.505338463935615,
7.19288116930449));
#12137=CARTESIAN_POINT('Ctrl Pts',(7.027329056784,-0.490739477737561,7.19382475428593));
#12138=CARTESIAN_POINT('Ctrl Pts',(7.03307700289468,-0.467352882771846,
7.1953405453573));
#12139=CARTESIAN_POINT('Ctrl Pts',(7.03516745610395,-0.458591888955015,
7.19590932656078));
#12140=CARTESIAN_POINT('Ctrl Pts',(7.03901510286803,-0.441968675865347,
7.19699045056201));
#12141=CARTESIAN_POINT('Ctrl Pts',(7.04078414514752,-0.434109362240635,
7.19750240277374));
#12142=CARTESIAN_POINT('Ctrl Pts',(7.04469197740838,-0.416243571726668,
7.1986680985766));
#12143=CARTESIAN_POINT('Ctrl Pts',(7.04680146308794,-0.406230983354801,
7.19932276112979));
#12144=CARTESIAN_POINT('Ctrl Pts',(7.05206423515512,-0.380262576897724,
7.20102441064051));
#12145=CARTESIAN_POINT('Ctrl Pts',(7.05509952620938,-0.364283885888679,
7.20207509821028));
#12146=CARTESIAN_POINT('Ctrl Pts',(7.0783285424351,-0.233281060990239,7.21072084935811));
#12147=CARTESIAN_POINT('Ctrl Pts',(7.08857715545971,-0.116744608515098,
7.21863090442123));
#12148=CARTESIAN_POINT('Ctrl Pts',(7.08857715545311,1.12752272796168E-10,
7.22671373997843));
#12149=CARTESIAN_POINT('Origin',(5.09382715545311,0.,-6.77268258743872));
#12150=CARTESIAN_POINT('',(7.08857666516212,-0.001398576294443,8.18540764972207));
#12151=CARTESIAN_POINT('',(7.08857712104368,-0.000272444087889267,8.02912895344979));
#12152=CARTESIAN_POINT('',(7.08857715545311,8.3550772080578E-14,-6.77268258743872));
#12153=CARTESIAN_POINT('Ctrl Pts',(7.08857708048265,-0.000546895445309948,
7.38540769765139));
#12154=CARTESIAN_POINT('Ctrl Pts',(7.08859597015781,0.0683514258463495,
7.38983115855148));
#12155=CARTESIAN_POINT('Ctrl Pts',(7.08504098529914,0.137392907239248,7.39425461945158));
#12156=CARTESIAN_POINT('Ctrl Pts',(7.0778937658154,0.206172859866408,7.39867808035167));
#12157=CARTESIAN_POINT('Ctrl Pts',(7.07063861570019,0.275991463081629,7.40316834022573));
#12158=CARTESIAN_POINT('Ctrl Pts',(7.0596817423248,0.345540058892286,7.40765860009979));
#12159=CARTESIAN_POINT('Ctrl Pts',(7.04505896197384,0.414393532432477,7.41214885997386));
#12160=CARTESIAN_POINT('Ctrl Pts',(7.03069092698795,0.482047500623273,7.41656089444458));
#12161=CARTESIAN_POINT('Ctrl Pts',(7.01278379571535,0.549029864948614,7.42097292891529));
#12162=CARTESIAN_POINT('Ctrl Pts',(6.99142365607376,0.614943154553544,7.42538496338601));
#12163=CARTESIAN_POINT('Ctrl Pts',(6.97007562037212,0.680819093723832,7.42979449773261));
#12164=CARTESIAN_POINT('Ctrl Pts',(6.94527860959919,0.745626687791695,7.43420403207922));
#12165=CARTESIAN_POINT('Ctrl Pts',(6.9171689403589,0.808982260569757,7.43861356642582));
#12166=CARTESIAN_POINT('Ctrl Pts',(6.88906532116135,0.87232419733101,7.44302215170856));
#12167=CARTESIAN_POINT('Ctrl Pts',(6.85765066061639,0.934214279254919,7.4474307369913));
#12168=CARTESIAN_POINT('Ctrl Pts',(6.82310921374251,0.99428925639292,7.45183932227404));
#12169=CARTESIAN_POINT('Ctrl Pts',(6.78745651537521,1.05629693798031,7.45638973852863));
#12170=CARTESIAN_POINT('Ctrl Pts',(6.74847263775237,1.11637021703044,7.46094015478322));
#12171=CARTESIAN_POINT('Ctrl Pts',(6.70641005089121,1.1741396713511,7.46549057103781));
#12172=CARTESIAN_POINT('Ctrl Pts',(6.6656075964235,1.23017843894577,7.46990466360539));
#12173=CARTESIAN_POINT('Ctrl Pts',(6.62190868633854,1.28404912791569,7.47431875617297));
#12174=CARTESIAN_POINT('Ctrl Pts',(6.57558479862159,1.33544818297521,7.47873284874055));
#12175=CARTESIAN_POINT('Ctrl Pts',(6.52711492855147,1.38922833061058,7.48335142683865));
#12176=CARTESIAN_POINT('Ctrl Pts',(6.4757713805736,1.44030182872507,7.48797000493674));
#12177=CARTESIAN_POINT('Ctrl Pts',(6.42190616946195,1.48836611593025,7.49258858303484));
#12178=CARTESIAN_POINT('Ctrl Pts',(6.36804095835031,1.53643040313543,7.49720716113293));
#12179=CARTESIAN_POINT('Ctrl Pts',(6.31165461331486,1.58148515758602,7.50182573923103));
#12180=CARTESIAN_POINT('Ctrl Pts',(6.25313367068357,1.62327938637938,7.50644431732912));
#12181=CARTESIAN_POINT('Ctrl Pts',(6.19667905707053,1.66359789342479,7.51089981702284));
#12182=CARTESIAN_POINT('Ctrl Pts',(6.13800773522275,1.70104701606772,7.51535531671655));
#12183=CARTESIAN_POINT('Ctrl Pts',(6.07744329185307,1.7353751348667,7.51981081641027));
#12184=CARTESIAN_POINT('Ctrl Pts',(6.01696941005075,1.76965192308176,7.52425965382801));
#12185=CARTESIAN_POINT('Ctrl Pts',(5.9546084474191,1.80081673092069,7.52870849124575));
#12186=CARTESIAN_POINT('Ctrl Pts',(5.89071401831209,1.82866040868795,7.5331573286635));
#12187=CARTESIAN_POINT('Ctrl Pts',(5.82689437395095,1.85647149703552,7.53760095897351));
#12188=CARTESIAN_POINT('Ctrl Pts',(5.76154527427762,1.88096898145218,7.54204458928353));
#12189=CARTESIAN_POINT('Ctrl Pts',(5.69504447026208,1.90198982722671,7.54648821959354));
#12190=CARTESIAN_POINT('Ctrl Pts',(5.62858524851718,1.92299752888199,7.5509290713471));
#12191=CARTESIAN_POINT('Ctrl Pts',(5.56097621645697,1.94053275748656,7.55536992310066));
#12192=CARTESIAN_POINT('Ctrl Pts',(5.49261319300565,1.95448132729713,7.55981077485422));
#12193=CARTESIAN_POINT('Ctrl Pts',(5.42426973105243,1.96842590584301,7.5642503558958));
#12194=CARTESIAN_POINT('Ctrl Pts',(5.35517318508442,1.97878576531309,7.56868993693738));
#12195=CARTESIAN_POINT('Ctrl Pts',(5.28573082354445,1.9854975559474,7.57312951797895));
#12196=CARTESIAN_POINT('Ctrl Pts',(5.21628478183528,1.99220970227993,7.57756933430068));
#12197=CARTESIAN_POINT('Ctrl Pts',(5.14649337530007,1.9952733512989,7.58200915062242));
#12198=CARTESIAN_POINT('Ctrl Pts',(5.07676849415664,1.99467705771505,7.58644896694415));
#12199=CARTESIAN_POINT('Ctrl Pts',(5.00697001312695,1.99408013469822,7.59089346982785));
#12200=CARTESIAN_POINT('Ctrl Pts',(4.9372386877492,1.98981556252933,7.59533797271155));
#12201=CARTESIAN_POINT('Ctrl Pts',(4.86798493486115,1.98192402828617,7.59978247559525));
#12202=CARTESIAN_POINT('Ctrl Pts',(4.79869055616879,1.97402786469207,7.604229585724));
#12203=CARTESIAN_POINT('Ctrl Pts',(4.72987479015126,1.96250058497032,7.60867669585275));
#12204=CARTESIAN_POINT('Ctrl Pts',(4.6619387061976,1.94743419141692,7.6131238059815));
#12205=CARTESIAN_POINT('Ctrl Pts',(4.59388533034977,1.93234178568066,7.61757859406194));
#12206=CARTESIAN_POINT('Ctrl Pts',(4.52671513938015,1.91369820030049,7.62203338214238));
#12207=CARTESIAN_POINT('Ctrl Pts',(4.46081408778557,1.89164532052447,7.62648817022282));
#12208=CARTESIAN_POINT('Ctrl Pts',(4.42736434458515,1.88045182440432,7.62874931042768));
#12209=CARTESIAN_POINT('Ctrl Pts',(4.39424125548785,1.86838075483627,7.63101045063254));
#12210=CARTESIAN_POINT('Ctrl Pts',(4.36149303308614,1.85545527990221,7.6332715908374));
#12211=CARTESIAN_POINT('Ctrl Pts',(4.29696377719709,1.82998607216092,7.63772709053111));
#12212=CARTESIAN_POINT('Ctrl Pts',(4.23363799911903,1.80109651306259,7.64218259022482));
#12213=CARTESIAN_POINT('Ctrl Pts',(4.17190279286082,1.76892143187842,7.64663808991853));
#12214=CARTESIAN_POINT('Ctrl Pts',(4.11025989880295,1.73679446185675,7.65108692733629));
#12215=CARTESIAN_POINT('Ctrl Pts',(4.05020328625875,1.70139194502923,7.65553576475404));
#12216=CARTESIAN_POINT('Ctrl Pts',(3.99210072440856,1.66289700030935,7.65998460217179));
#12217=CARTESIAN_POINT('Ctrl Pts',(3.93406616825767,1.62444711170322,7.66442823248181));
#12218=CARTESIAN_POINT('Ctrl Pts',(3.8779815260734,1.58291225306713,7.66887186279182));
#12219=CARTESIAN_POINT('Ctrl Pts',(3.82418898030399,1.5385208697655,7.67331549310184));
#12220=CARTESIAN_POINT('Ctrl Pts',(3.77043007046165,1.49415724394051,7.6777563448554));
#12221=CARTESIAN_POINT('Ctrl Pts',(3.7189607901727,1.44694094754962,7.68219719660896));
#12222=CARTESIAN_POINT('Ctrl Pts',(3.67009214155776,1.39714214477569,7.68663804836252));
#12223=CARTESIAN_POINT('Ctrl Pts',(3.6212374762912,1.34735759150583,7.6910776294041));
#12224=CARTESIAN_POINT('Ctrl Pts',(3.57498230781504,1.29499234785888,7.69551721044568));
#12225=CARTESIAN_POINT('Ctrl Pts',(3.53160119245343,1.24035382170964,7.69995679148727));
#12226=CARTESIAN_POINT('Ctrl Pts',(3.4882177780651,1.18571239993566,7.704396607809));
#12227=CARTESIAN_POINT('Ctrl Pts',(3.44770902145391,1.12879784108382,7.70883642413074));
#12228=CARTESIAN_POINT('Ctrl Pts',(3.41030842487547,1.06994964661626,7.71327624045247));
#12229=CARTESIAN_POINT('Ctrl Pts',(3.37286834913832,1.01103933342808,7.71772074333617));
#12230=CARTESIAN_POINT('Ctrl Pts',(3.33854324457653,0.950191724505961,7.72216524621986));
#12231=CARTESIAN_POINT('Ctrl Pts',(3.30752205488232,0.887773422768894,7.72660974910356));
#12232=CARTESIAN_POINT('Ctrl Pts',(3.27648266746263,0.825318505056366,7.73105685923231));
#12233=CARTESIAN_POINT('Ctrl Pts',(3.24875124706848,0.761291509552212,7.73550396936107));
#12234=CARTESIAN_POINT('Ctrl Pts',(3.22446858451634,0.696079087291983,7.73995107948982));
#12235=CARTESIAN_POINT('Ctrl Pts',(3.20014399785965,0.630754075549302,7.74440586757026));
#12236=CARTESIAN_POINT('Ctrl Pts',(3.17928020063015,0.564240018419293,7.7488606556507));
#12237=CARTESIAN_POINT('Ctrl Pts',(3.16196789788011,0.496937995558288,7.75331544373114));
#12238=CARTESIAN_POINT('Ctrl Pts',(3.1531806013624,0.462777154007605,7.75557658393598));
#12239=CARTESIAN_POINT('Ctrl Pts',(3.14530746504828,0.428413459846191,7.75783772414082));
#12240=CARTESIAN_POINT('Ctrl Pts',(3.1383552500829,0.393899974368878,7.76009886434566));
#12241=CARTESIAN_POINT('Ctrl Pts',(3.1246561474874,0.325892327764686,7.76455436403937));
#12242=CARTESIAN_POINT('Ctrl Pts',(3.11448212774918,0.257035591591292,7.76900986373308));
#12243=CARTESIAN_POINT('Ctrl Pts',(3.10793043782018,0.187727966469484,7.77346536342679));
#12244=CARTESIAN_POINT('Ctrl Pts',(3.101388544585,0.118523976530287,7.77791420084455));
#12245=CARTESIAN_POINT('Ctrl Pts',(3.09845827621122,0.0488709189142223,
7.7823630382623));
#12246=CARTESIAN_POINT('Ctrl Pts',(3.09918584280205,-0.0208229768686858,
7.78681187568006));
#12247=CARTESIAN_POINT('Ctrl Pts',(3.09991255781813,-0.0904352999641432,
7.79125550599008));
#12248=CARTESIAN_POINT('Ctrl Pts',(3.10428859934531,-0.160087879467095,
7.79569913630009));
#12249=CARTESIAN_POINT('Ctrl Pts',(3.11230822396324,-0.229369323684002,
7.80014276661011));
#12250=CARTESIAN_POINT('Ctrl Pts',(3.12032283399215,-0.29860744692438,7.80458361836366));
#12251=CARTESIAN_POINT('Ctrl Pts',(3.13197645120835,-0.367474410441749,
7.80902447011722));
#12252=CARTESIAN_POINT('Ctrl Pts',(3.14721136618868,-0.435562316421431,
7.81346532187078));
#12253=CARTESIAN_POINT('Ctrl Pts',(3.16244192182759,-0.503630739625652,
7.81790490291236));
#12254=CARTESIAN_POINT('Ctrl Pts',(3.18125163405266,-0.57092007071881,7.82234448395394));
#12255=CARTESIAN_POINT('Ctrl Pts',(3.20353172145893,-0.637032757965206,
7.82678406499552));
#12256=CARTESIAN_POINT('Ctrl Pts',(3.22581298962126,-0.703148948921208,
7.83122388131724));
#12257=CARTESIAN_POINT('Ctrl Pts',(3.25156483958468,-0.768087909452814,
7.83566369763897));
#12258=CARTESIAN_POINT('Ctrl Pts',(3.28062923577066,-0.831469101385753,
7.8401035139607));
#12259=CARTESIAN_POINT('Ctrl Pts',(3.30972431162534,-0.894917196961157,
7.84454801684439));
#12260=CARTESIAN_POINT('Ctrl Pts',(3.34213870825378,-0.956803796527888,
7.84899251972809));
#12261=CARTESIAN_POINT('Ctrl Pts',(3.37766742110722,-1.01677103062088,7.85343702261179));
#12262=CARTESIAN_POINT('Ctrl Pts',(3.41321697590028,-1.07677344283803,7.85788413274054));
#12263=CARTESIAN_POINT('Ctrl Pts',(3.45188421208295,-1.13485384122124,7.86233124286929));
#12264=CARTESIAN_POINT('Ctrl Pts',(3.49342112260742,-1.19068387598519,7.86677835299803));
#12265=CARTESIAN_POINT('Ctrl Pts',(3.53502974675788,-1.24661030150574,7.87123314107848));
#12266=CARTESIAN_POINT('Ctrl Pts',(3.57951762271077,-1.30027823163097,7.87568792915892));
#12267=CARTESIAN_POINT('Ctrl Pts',(3.62659740700095,-1.35139351328804,7.88014271723936));
#12268=CARTESIAN_POINT('Ctrl Pts',(3.65049394061156,-1.37733836551178,7.88240385744417));
#12269=CARTESIAN_POINT('Ctrl Pts',(3.6750576598063,-1.40262617781603,7.88466499764899));
#12270=CARTESIAN_POINT('Ctrl Pts',(3.70024770244873,-1.42722243209109,7.8869261378538));
#12271=CARTESIAN_POINT('Ctrl Pts',(3.74988382277378,-1.47568851267988,7.89138163754751));
#12272=CARTESIAN_POINT('Ctrl Pts',(3.80214879930399,-1.52165733931686,7.89583713724122));
#12273=CARTESIAN_POINT('Ctrl Pts',(3.856761261163,-1.56483083292866,7.90029263693493));
#12274=CARTESIAN_POINT('Ctrl Pts',(3.91129206140881,-1.60793976953249,7.90474147435267));
#12275=CARTESIAN_POINT('Ctrl Pts',(3.96816299928352,-1.64826136837502,7.9091903117704));
#12276=CARTESIAN_POINT('Ctrl Pts',(4.02705654344727,-1.68553493700389,7.91363914918814));
#12277=CARTESIAN_POINT('Ctrl Pts',(4.08588115611273,-1.72276487906945,7.91808277949815));
#12278=CARTESIAN_POINT('Ctrl Pts',(4.1467232617324,-1.75695361631742,7.92252640980815));
#12279=CARTESIAN_POINT('Ctrl Pts',(4.20923443383318,-1.78788234494249,7.92697004011816));
#12280=CARTESIAN_POINT('Ctrl Pts',(4.27170651833915,-1.81879173415075,7.9314108918717));
#12281=CARTESIAN_POINT('Ctrl Pts',(4.33584516144208,-1.84644494226885,7.93585174362526));
#12282=CARTESIAN_POINT('Ctrl Pts',(4.401276621564,-1.87066868272014,7.94029259537881));
#12283=CARTESIAN_POINT('Ctrl Pts',(4.46668935903,-1.89488549175409,7.94473217642039));
#12284=CARTESIAN_POINT('Ctrl Pts',(4.53339372059257,-1.91567461154033,7.94917175746196));
#12285=CARTESIAN_POINT('Ctrl Pts',(4.60099688698302,-1.93291124705189,7.95361133850354));
#12286=CARTESIAN_POINT('Ctrl Pts',(4.66860363607269,-1.95014879603665,7.95805115482528));
#12287=CARTESIAN_POINT('Ctrl Pts',(4.73710880995683,-1.96383336846661,7.96249097114702));
#12288=CARTESIAN_POINT('Ctrl Pts',(4.80610709619892,-1.97389075938938,7.96693078746875));
#12289=CARTESIAN_POINT('Ctrl Pts',(4.87517821535117,-1.983958766649,7.97137529035244));
#12290=CARTESIAN_POINT('Ctrl Pts',(4.94474300074929,-1.99039187998696,7.97581979323614));
#12291=CARTESIAN_POINT('Ctrl Pts',(5.01438963566877,-1.99316764045338,7.98026429611983));
#12292=CARTESIAN_POINT('Ctrl Pts',(5.08407712686621,-1.99594502924315,7.98471140624858));
#12293=CARTESIAN_POINT('Ctrl Pts',(5.15384607390411,-1.9950608009897,7.98915851637734));
#12294=CARTESIAN_POINT('Ctrl Pts',(5.22328606227653,-1.9905446375161,7.9936056265061));
#12295=CARTESIAN_POINT('Ctrl Pts',(5.29284593903943,-1.98602067686996,7.99806041458654));
#12296=CARTESIAN_POINT('Ctrl Pts',(5.3620752377972,-1.9778523218194,8.00251520266698));
#12297=CARTESIAN_POINT('Ctrl Pts',(5.43057086477357,-1.9661208601541,8.00696999074742));
#12298=CARTESIAN_POINT('Ctrl Pts',(5.46533755024061,-1.96016626048415,8.00923113095231));
#12299=CARTESIAN_POINT('Ctrl Pts',(5.49991541391814,-1.95329449976434,8.01149227115719));
#12300=CARTESIAN_POINT('Ctrl Pts',(5.53425327092352,-1.945521112533,8.01375341136208));
#12301=CARTESIAN_POINT('Ctrl Pts',(5.60191484760934,-1.93020391798067,8.01820891105579));
#12302=CARTESIAN_POINT('Ctrl Pts',(5.66890933243172,-1.91132271575537,8.0226644107495));
#12303=CARTESIAN_POINT('Ctrl Pts',(5.73483358288269,-1.88895164641501,8.02711991044321));
#12304=CARTESIAN_POINT('Ctrl Pts',(5.8006592572862,-1.8666140283703,8.03156874786096));
#12305=CARTESIAN_POINT('Ctrl Pts',(5.8654174141304,-1.84079705662434,8.03601758527871));
#12306=CARTESIAN_POINT('Ctrl Pts',(5.928716635496,-1.81162554591552,8.04046642269646));
#12307=CARTESIAN_POINT('Ctrl Pts',(5.99194176877194,-1.78248817877837,8.04491005300647));
#12308=CARTESIAN_POINT('Ctrl Pts',(6.0537109160025,-1.75000427474488,8.04935368331648));
#12309=CARTESIAN_POINT('Ctrl Pts',(6.11365102479551,-1.71434735045716,8.05379731362648));
#12310=CARTESIAN_POINT('Ctrl Pts',(6.17355365365331,-1.67871272207847,8.05823816538004));
#12311=CARTESIAN_POINT('Ctrl Pts',(6.23162909350217,-1.63990925902836,8.06267901713359));
#12312=CARTESIAN_POINT('Ctrl Pts',(6.28752873634795,-1.59815646864416,8.06711986888714));
#12313=CARTESIAN_POINT('Ctrl Pts',(6.3434123839861,-1.556415625466,8.07155944992872));
#12314=CARTESIAN_POINT('Ctrl Pts',(6.39712107889992,-1.51172742295573,8.0759990309703));
#12315=CARTESIAN_POINT('Ctrl Pts',(6.44833654454803,-1.46435374051276,8.08043861201187));
#12316=CARTESIAN_POINT('Ctrl Pts',(6.49955472441234,-1.41697754745283,8.0848784283336));
#12317=CARTESIAN_POINT('Ctrl Pts',(6.5482790552334,-1.36691592584987,8.08931824465534));
#12318=CARTESIAN_POINT('Ctrl Pts',(6.59422693255357,-1.3144687411182,8.09375806097707));
#12319=CARTESIAN_POINT('Ctrl Pts',(6.64022331133381,-1.26196619441589,8.09820256386076));
#12320=CARTESIAN_POINT('Ctrl Pts',(6.68343706422757,-1.20707342735552,8.10264706674445));
#12321=CARTESIAN_POINT('Ctrl Pts',(6.7236254845366,-1.15012389289879,8.10709156962815));
#12322=CARTESIAN_POINT('Ctrl Pts',(6.76383748027423,-1.09314095056801,8.1115386797569));
#12323=CARTESIAN_POINT('Ctrl Pts',(6.80102035026782,-1.03409925335822,8.11598578988566));
#12324=CARTESIAN_POINT('Ctrl Pts',(6.83497591475613,-0.973359419987069,
8.12043290001441));
#12325=CARTESIAN_POINT('Ctrl Pts',(6.868990103649,-0.912514719074521,8.12488768809484));
#12326=CARTESIAN_POINT('Ctrl Pts',(6.89976564909241,-0.849966468632431,
8.12934247617528));
#12327=CARTESIAN_POINT('Ctrl Pts',(6.92715166655712,-0.786097194680931,
8.13379726425571));
#12328=CARTESIAN_POINT('Ctrl Pts',(6.94105213141024,-0.753678731539992,
8.13605840446056));
#12329=CARTESIAN_POINT('Ctrl Pts',(6.95408013091807,-0.720920206227092,
8.13831954466541));
#12330=CARTESIAN_POINT('Ctrl Pts',(6.96622088098836,-0.687873025402394,
8.14058068487025));
#12331=CARTESIAN_POINT('Ctrl Pts',(6.99377560713267,-0.612868926628099,
8.1457125835386));
#12332=CARTESIAN_POINT('Ctrl Pts',(7.01684654224403,-0.536134208834767,
8.15084448220696));
#12333=CARTESIAN_POINT('Ctrl Pts',(7.0352446347772,-0.458176530907991,8.15597638087531));
#12334=CARTESIAN_POINT('Ctrl Pts',(7.05348683700635,-0.380879402225201,
8.16106479605523));
#12335=CARTESIAN_POINT('Ctrl Pts',(7.06713495375901,-0.302380129726197,
8.16615321123516));
#12336=CARTESIAN_POINT('Ctrl Pts',(7.07605109270582,-0.223194590172708,
8.17124162641508));
#12337=CARTESIAN_POINT('Ctrl Pts',(7.0843251968989,-0.149711055566642,8.17596363418408));
#12338=CARTESIAN_POINT('Ctrl Pts',(7.08852461457797,-0.0756368410426775,
8.18068564195308));
#12339=CARTESIAN_POINT('Ctrl Pts',(7.08857666516212,-0.001398576294443,
8.18540764972207));
#12340=CARTESIAN_POINT('Ctrl Pts',(7.08857715545311,1.12756902441053E-10,
7.22671373997843));
#12341=CARTESIAN_POINT('Ctrl Pts',(7.08857715545308,0.000600191909874145,
7.22675529437358));
#12342=CARTESIAN_POINT('Ctrl Pts',(7.08857688458501,0.001200389246813,7.2267968527846));
#12343=CARTESIAN_POINT('Ctrl Pts',(7.08846930109933,0.120384606063082,7.23505003639251));
#12344=CARTESIAN_POINT('Ctrl Pts',(7.07778833453187,0.238722052384156,7.24340464028335));
#12345=CARTESIAN_POINT('Ctrl Pts',(7.0483933295436,0.401062417775733,7.2546634015799));
#12346=CARTESIAN_POINT('Ctrl Pts',(7.03853620442267,0.446416242704073,7.25778379811172));
#12347=CARTESIAN_POINT('Ctrl Pts',(7.02492514741938,0.499966438045238,7.26140695740263));
#12348=CARTESIAN_POINT('Ctrl Pts',(7.02268779594919,0.508529773151547,7.26198445172257));
#12349=CARTESIAN_POINT('Ctrl Pts',(7.01893366488793,0.522517180831181,7.26292431479112));
#12350=CARTESIAN_POINT('Ctrl Pts',(7.01745080708027,0.527950116687992,7.26328852514501));
#12351=CARTESIAN_POINT('Ctrl Pts',(7.01474251371937,0.537709931944364,7.2639411816215));
#12352=CARTESIAN_POINT('Ctrl Pts',(7.01352544340598,0.542038992091794,7.26423009324422));
#12353=CARTESIAN_POINT('Ctrl Pts',(7.01081919381303,0.551541537905058,7.26486299271094));
#12354=CARTESIAN_POINT('Ctrl Pts',(7.00932370929607,0.556713119141431,7.26520661324837));
#12355=CARTESIAN_POINT('Ctrl Pts',(7.00496192540704,0.571571073988756,7.26619163387933));
#12356=CARTESIAN_POINT('Ctrl Pts',(7.00204291190497,0.581241979285742,7.26683007711997));
#12357=CARTESIAN_POINT('Ctrl Pts',(6.98031705892309,0.651293198308156,7.2714378283084));
#12358=CARTESIAN_POINT('Ctrl Pts',(6.95871963766281,0.71077756033698,7.27525995311493));
#12359=CARTESIAN_POINT('Ctrl Pts',(6.88373654286131,0.890207073890386,7.28679238951352));
#12360=CARTESIAN_POINT('Ctrl Pts',(6.82132055658072,1.00598883967134,7.29425803174684));
#12361=CARTESIAN_POINT('Ctrl Pts',(6.6984808400835,1.18825925284503,7.30719065598847));
#12362=CARTESIAN_POINT('Ctrl Pts',(6.64414592038585,1.25832522383765,7.31249906724981));
#12363=CARTESIAN_POINT('Ctrl Pts',(6.57495116503624,1.33624249689079,7.31896634895358));
#12364=CARTESIAN_POINT('Ctrl Pts',(6.56442532463618,1.347817994155,7.31994277350658));
#12365=CARTESIAN_POINT('Ctrl Pts',(6.54691962807049,1.36662018644199,7.32155546264852));
#12366=CARTESIAN_POINT('Ctrl Pts',(6.54001928463785,1.37392022604434,7.32218836516292));
#12367=CARTESIAN_POINT('Ctrl Pts',(6.52749887922954,1.38696703480958,7.32333195418898));
#12368=CARTESIAN_POINT('Ctrl Pts',(6.52189862729725,1.39273257857758,7.32384178024818));
#12369=CARTESIAN_POINT('Ctrl Pts',(6.50986694905094,1.40497050447237,7.32493361021595));
#12370=CARTESIAN_POINT('Ctrl Pts',(6.50342567147932,1.41143290118953,7.32551603937571));
#12371=CARTESIAN_POINT('Ctrl Pts',(6.48584348276125,1.42883233524096,7.32710036618503));
#12372=CARTESIAN_POINT('Ctrl Pts',(6.47461832589639,1.43968295761348,7.3281059901386));
#12373=CARTESIAN_POINT('Ctrl Pts',(6.41403096413897,1.49688837313351,7.33350402032759));
#12374=CARTESIAN_POINT('Ctrl Pts',(6.36246492436985,1.54083397270196,7.3379967066575));
#12375=CARTESIAN_POINT('Ctrl Pts',(6.17799495329815,1.682496773064,7.35373829720515));
#12376=CARTESIAN_POINT('Ctrl Pts',(6.03529388424404,1.76630838208587,7.3654295189683));
#12377=CARTESIAN_POINT('Ctrl Pts',(5.83481356114489,1.85278898690861,7.38039672863195));
#12378=CARTESIAN_POINT('Ctrl Pts',(5.7848687125538,1.87199106464918,7.38400924316252));
#12379=CARTESIAN_POINT('Ctrl Pts',(5.72548266043479,1.89212149819018,7.38812420732276));
#12380=CARTESIAN_POINT('Ctrl Pts',(5.71673678756077,1.89501874366896,7.38872570927152));
#12381=CARTESIAN_POINT('Ctrl Pts',(5.70250861971097,1.89962296236539,7.38969659325848));
#12382=CARTESIAN_POINT('Ctrl Pts',(5.69703859263579,1.90136700510846,7.39006802040016));
#12383=CARTESIAN_POINT('Ctrl Pts',(5.68726464021795,1.90443687060614,7.3907283379507));
#12384=CARTESIAN_POINT('Ctrl Pts',(5.68296368896756,1.90577175670558,7.39101774437718));
#12385=CARTESIAN_POINT('Ctrl Pts',(5.67359471356587,1.90864485699751,7.39164563756338));
#12386=CARTESIAN_POINT('Ctrl Pts',(5.66852507578857,1.91017745602564,7.39198379872935));
#12387=CARTESIAN_POINT('Ctrl Pts',(5.65416064776527,1.91445759412602,7.39293759477621));
#12388=CARTESIAN_POINT('Ctrl Pts',(5.64485170124714,1.91715765163288,7.39355055719189));
#12389=CARTESIAN_POINT('Ctrl Pts',(5.58457301697503,1.93416614183261,7.39748870606577));
#12390=CARTESIAN_POINT('Ctrl Pts',(5.53306566810787,1.94650989444179,7.40071117194312));
#12391=CARTESIAN_POINT('Ctrl Pts',(5.316016896263,1.98946911779409,7.41393018360304));
#12392=CARTESIAN_POINT('Ctrl Pts',(5.1474344918077,2.00112184492285,7.42339052563864));
#12393=CARTESIAN_POINT('Ctrl Pts',(4.91459359733022,1.98774101111655,7.43728752965647));
#12394=CARTESIAN_POINT('Ctrl Pts',(4.8500310272001,1.98085869272376,7.44122235796352));
#12395=CARTESIAN_POINT('Ctrl Pts',(4.77024006774156,1.96839297826526,7.44624286507685));
#12396=CARTESIAN_POINT('Ctrl Pts',(4.75458730219337,1.96575578833853,7.44723527352566));
#12397=CARTESIAN_POINT('Ctrl Pts',(4.72984233003675,1.96128238897049,7.44881679696032));
#12398=CARTESIAN_POINT('Ctrl Pts',(4.72072837970652,1.95956904988819,7.44940202732317));
#12399=CARTESIAN_POINT('Ctrl Pts',(4.70375271560743,1.95625505967262,7.45049732163637));
#12400=CARTESIAN_POINT('Ctrl Pts',(4.69588804213954,1.95467040345492,7.45100686837202));
#12401=CARTESIAN_POINT('Ctrl Pts',(4.67840016082486,1.95103684660869,7.4521446887413));
#12402=CARTESIAN_POINT('Ctrl Pts',(4.66878217230397,1.94896411492892,7.45277370952778));
#12403=CARTESIAN_POINT('Ctrl Pts',(4.64066144006187,1.94268588033353,7.45462252927555));
#12404=CARTESIAN_POINT('Ctrl Pts',(4.62220331534612,1.93828751932807,7.45584843802616));
#12405=CARTESIAN_POINT('Ctrl Pts',(4.48260811133525,1.90291157444481,7.46521664367364));
#12406=CARTESIAN_POINT('Ctrl Pts',(4.36458306180081,1.86087455792052,7.4737202764263));
#12407=CARTESIAN_POINT('Ctrl Pts',(4.1273376369796,1.75032134594481,7.49188857337727));
#12408=CARTESIAN_POINT('Ctrl Pts',(4.00965262147061,1.67996900407864,7.50154024703534));
#12409=CARTESIAN_POINT('Ctrl Pts',(3.88165289119638,1.58435807810279,7.51222073634554));
#12410=CARTESIAN_POINT('Ctrl Pts',(3.8634576690243,1.57027004122678,7.51374293388061));
#12411=CARTESIAN_POINT('Ctrl Pts',(3.83948962705213,1.55103980990285,7.51574901237472));
#12412=CARTESIAN_POINT('Ctrl Pts',(3.83349783549211,1.54617500206067,7.51625059187154));
#12413=CARTESIAN_POINT('Ctrl Pts',(3.82415117335156,1.53849590005424,7.51703293252671));
#12414=CARTESIAN_POINT('Ctrl Pts',(3.82077715485614,1.53570519009544,7.51731533063023));
#12415=CARTESIAN_POINT('Ctrl Pts',(3.81390526705266,1.52998312058331,7.51789041106131));
#12416=CARTESIAN_POINT('Ctrl Pts',(3.81040825976877,1.5270508597377,7.51818300937065));
#12417=CARTESIAN_POINT('Ctrl Pts',(3.80215239364931,1.5200798759383,7.51887372916558));
#12418=CARTESIAN_POINT('Ctrl Pts',(3.79740232621506,1.51603073324984,7.51927109843413));
#12419=CARTESIAN_POINT('Ctrl Pts',(3.78162170816747,1.50245031203677,7.52059140226085));
#12420=CARTESIAN_POINT('Ctrl Pts',(3.770676341725,1.49282015971812,7.52150743574005));
#12421=CARTESIAN_POINT('Ctrl Pts',(3.70966727997524,1.43794382381555,7.52662150516241));
#12422=CARTESIAN_POINT('Ctrl Pts',(3.66181414125883,1.39029551515154,7.53066467284083));
#12423=CARTESIAN_POINT('Ctrl Pts',(3.50176865881665,1.21388442307065,7.54470041148724));
#12424=CARTESIAN_POINT('Ctrl Pts',(3.40377855382796,1.07326733954188,7.55433997793486));
#12425=CARTESIAN_POINT('Ctrl Pts',(3.30451813096039,0.882804188253043,7.56732597241304));
#12426=CARTESIAN_POINT('Ctrl Pts',(3.28545151715098,0.843058201071235,7.5700277931325));
#12427=CARTESIAN_POINT('Ctrl Pts',(3.26203940070591,0.789797632278761,7.57365434516304));
#12428=CARTESIAN_POINT('Ctrl Pts',(3.25649834857213,0.776820132121396,7.57453841837982));
#12429=CARTESIAN_POINT('Ctrl Pts',(3.24772797026515,0.755660448273479,7.57598107488438));
#12430=CARTESIAN_POINT('Ctrl Pts',(3.24441419772565,0.747513626916368,7.57653680211545));
#12431=CARTESIAN_POINT('Ctrl Pts',(3.23814911312386,0.731814397028634,7.57760837056788));
#12432=CARTESIAN_POINT('Ctrl Pts',(3.23518975720093,0.724265370652425,7.57812392938153));
#12433=CARTESIAN_POINT('Ctrl Pts',(3.22845157753333,0.706763644744733,7.57931997970669));
#12434=CARTESIAN_POINT('Ctrl Pts',(3.22470626769621,0.696798389737538,7.580001571668));
#12435=CARTESIAN_POINT('Ctrl Pts',(3.21307895282669,0.665092864707059,7.58217221998937));
#12436=CARTESIAN_POINT('Ctrl Pts',(3.20549537075811,0.643245922617052,7.5836710482719));
#12437=CARTESIAN_POINT('Ctrl Pts',(3.16887203689989,0.531506348518307,7.5913557999887));
#12438=CARTESIAN_POINT('Ctrl Pts',(3.14586828773197,0.439776077536353,7.59773403576874));
#12439=CARTESIAN_POINT('Ctrl Pts',(3.10938169734766,0.233089039633766,7.61219694062287));
#12440=CARTESIAN_POINT('Ctrl Pts',(3.09922025961846,0.117882804479479,7.62032354062417));
#12441=CARTESIAN_POINT('Ctrl Pts',(3.09905898623916,-0.0135881838842559,
7.62938162180226));
#12442=CARTESIAN_POINT('Ctrl Pts',(3.09923266791226,-0.0296232678572957,
7.63048243732483));
#12443=CARTESIAN_POINT('Ctrl Pts',(3.10070229976475,-0.0938175958722112,
7.63486961836063));
#12444=CARTESIAN_POINT('Ctrl Pts',(3.10354943996742,-0.141929141577623,
7.63811334000337));
#12445=CARTESIAN_POINT('Ctrl Pts',(3.10898784104279,-0.198797508202418,
7.64186018613473));
#12446=CARTESIAN_POINT('Ctrl Pts',(3.10989914782426,-0.207695019061908,
7.64244385633825));
#12447=CARTESIAN_POINT('Ctrl Pts',(3.11148482923736,-0.222212732893909,
7.6433917091354));
#12448=CARTESIAN_POINT('Ctrl Pts',(3.11212332384377,-0.227836613952299,
7.64375778483184));
#12449=CARTESIAN_POINT('Ctrl Pts',(3.11331221260484,-0.237925109660984,
7.64441240161624));
#12450=CARTESIAN_POINT('Ctrl Pts',(3.11385377702376,-0.242390632215528,
7.64470142130376));
#12451=CARTESIAN_POINT('Ctrl Pts',(3.11507373683139,-0.252172951390316,
7.64533293744749));
#12452=CARTESIAN_POINT('Ctrl Pts',(3.1157584557532,-0.257488854138161,7.64567507781246));
#12453=CARTESIAN_POINT('Ctrl Pts',(3.11778073763001,-0.272704812716511,
7.64665159452664));
#12454=CARTESIAN_POINT('Ctrl Pts',(3.11917127810093,-0.282597834558267,
7.64728309280997));
#12455=CARTESIAN_POINT('Ctrl Pts',(3.12945229288826,-0.351957756811089,
7.65168921556053));
#12456=CARTESIAN_POINT('Ctrl Pts',(3.14095415393568,-0.4110126672403,7.65533092965514));
#12457=CARTESIAN_POINT('Ctrl Pts',(3.17683776130088,-0.559199402976622,
7.66439188835514));
#12458=CARTESIAN_POINT('Ctrl Pts',(3.20477253058801,-0.647322581658998,
7.66971147220542));
#12459=CARTESIAN_POINT('Ctrl Pts',(3.28637826284454,-0.853799134393472,
7.68261682854989));
#12460=CARTESIAN_POINT('Ctrl Pts',(3.34568332038866,-0.969448930436627,
7.69023426476554));
#12461=CARTESIAN_POINT('Ctrl Pts',(3.4245543767293,-1.09216253350547,7.69928041885801));
#12462=CARTESIAN_POINT('Ctrl Pts',(3.43348935738593,-1.10569841348626,7.70029202123762));
#12463=CARTESIAN_POINT('Ctrl Pts',(3.44832124857513,-1.12758250026291,7.70195095958232));
#12464=CARTESIAN_POINT('Ctrl Pts',(3.45411912372077,-1.13599716061122,7.70259459130304));
#12465=CARTESIAN_POINT('Ctrl Pts',(3.46460209568651,-1.15096400559889,7.70374992511146));
#12466=CARTESIAN_POINT('Ctrl Pts',(3.46926273877118,-1.15753310557866,7.70426069080376));
#12467=CARTESIAN_POINT('Ctrl Pts',(3.47922387408791,-1.17139450104773,7.70534637675932));
#12468=CARTESIAN_POINT('Ctrl Pts',(3.48453425931719,-1.17867943196744,7.70592166965179));
#12469=CARTESIAN_POINT('Ctrl Pts',(3.49887886925119,-1.19808010247063,7.70746654768593));
#12470=CARTESIAN_POINT('Ctrl Pts',(3.50800156811642,-1.2101293952983,7.70843954912044));
#12471=CARTESIAN_POINT('Ctrl Pts',(3.55440252110325,-1.26999012228401,7.71334273963552));
#12472=CARTESIAN_POINT('Ctrl Pts',(3.59370643402031,-1.31618374394274,7.71735248324679));
#12473=CARTESIAN_POINT('Ctrl Pts',(3.72219952978876,-1.45395748255061,7.73004589455525));
#12474=CARTESIAN_POINT('Ctrl Pts',(3.81811925593308,-1.53880385495083,7.7389786311471));
#12475=CARTESIAN_POINT('Ctrl Pts',(4.00009499929227,-1.67099354149216,7.75463566391836));
#12476=CARTESIAN_POINT('Ctrl Pts',(4.082788992514,-1.72228793169034,7.76134804747826));
#12477=CARTESIAN_POINT('Ctrl Pts',(4.17856517640783,-1.77241136158735,7.76845251611215));
#12478=CARTESIAN_POINT('Ctrl Pts',(4.18827038008275,-1.77738950833605,7.76916506839146));
#12479=CARTESIAN_POINT('Ctrl Pts',(4.20304024411531,-1.7848131159357,7.77023781296761));
#12480=CARTESIAN_POINT('Ctrl Pts',(4.20807503233778,-1.78731708392591,7.77060145780591));
#12481=CARTESIAN_POINT('Ctrl Pts',(4.2171549500782,-1.79178503889408,7.77125352291199));
#12482=CARTESIAN_POINT('Ctrl Pts',(4.22119617175201,-1.79375665817198,7.77154240470188));
#12483=CARTESIAN_POINT('Ctrl Pts',(4.23009697626533,-1.79806195658588,7.7721757367278));
#12484=CARTESIAN_POINT('Ctrl Pts',(4.23495935952318,-1.80038960586883,7.77251981619273));
#12485=CARTESIAN_POINT('Ctrl Pts',(4.24899141502858,-1.80703704311368,7.77350747950672));
#12486=CARTESIAN_POINT('Ctrl Pts',(4.25818481314968,-1.81130676293157,7.77414808181425));
#12487=CARTESIAN_POINT('Ctrl Pts',(4.32590243563476,-1.84213175348497,7.77882212642475));
#12488=CARTESIAN_POINT('Ctrl Pts',(4.38565345086151,-1.86591789088091,7.78270352559359));
#12489=CARTESIAN_POINT('Ctrl Pts',(4.57596206307224,-1.93121462403671,7.79462719138739));
#12490=CARTESIAN_POINT('Ctrl Pts',(4.70970219905284,-1.96219901981723,7.80240512551316));
#12491=CARTESIAN_POINT('Ctrl Pts',(4.9271840764416,-1.98947831170805,7.81533992358522));
#12492=CARTESIAN_POINT('Ctrl Pts',(5.00934827425976,-1.994656563911,7.82028474325504));
#12493=CARTESIAN_POINT('Ctrl Pts',(5.10699659190726,-1.99476601414574,7.82634703418628));
#12494=CARTESIAN_POINT('Ctrl Pts',(5.1224011998441,-1.99460482013604,7.82730871462794));
#12495=CARTESIAN_POINT('Ctrl Pts',(5.14777159253123,-1.99404538563801,7.82890199393496));
#12496=CARTESIAN_POINT('Ctrl Pts',(5.15773918133644,-1.99375079923028,7.8295303697587));
#12497=CARTESIAN_POINT('Ctrl Pts',(5.1757302081478,-1.99308403259137,7.8306690755864));
#12498=CARTESIAN_POINT('Ctrl Pts',(5.18375444993668,-1.99273810362685,7.83117857718081));
#12499=CARTESIAN_POINT('Ctrl Pts',(5.2009398908741,-1.99189321976894,7.83227334636384));
#12500=CARTESIAN_POINT('Ctrl Pts',(5.21010014677491,-1.99137950273603,7.83285906297571));
#12501=CARTESIAN_POINT('Ctrl Pts',(5.23506781679531,-1.98980643056041,7.83446162202954));
#12502=CARTESIAN_POINT('Ctrl Pts',(5.25086640514954,-1.9886219363252,7.83548233790329));
#12503=CARTESIAN_POINT('Ctrl Pts',(5.33775551433902,-1.98106560135035,7.84113413887891));
#12504=CARTESIAN_POINT('Ctrl Pts',(5.40847084081499,-1.97107058257865,7.84587716745047));
#12505=CARTESIAN_POINT('Ctrl Pts',(5.6726362358696,-1.91915486044602,7.86413779330567));
#12506=CARTESIAN_POINT('Ctrl Pts',(5.85999553274186,-1.85233605605529,7.87833316509535));
#12507=CARTESIAN_POINT('Ctrl Pts',(6.05345619596284,-1.74888660180752,7.89297430662287));
#12508=CARTESIAN_POINT('Ctrl Pts',(6.07230043743263,-1.73841375062501,7.89439864503102));
#12509=CARTESIAN_POINT('Ctrl Pts',(6.09748686678872,-1.72387683068597,7.89629622203952));
#12510=CARTESIAN_POINT('Ctrl Pts',(6.1039804474656,-1.72007978725546,7.89678489665242));
#12511=CARTESIAN_POINT('Ctrl Pts',(6.1141862787711,-1.71403432129829,7.89755186280676));
#12512=CARTESIAN_POINT('Ctrl Pts',(6.11791285585614,-1.71181040837794,7.8978316868636));
#12513=CARTESIAN_POINT('Ctrl Pts',(6.12548242906986,-1.70725954134041,7.89839956584807));
#12514=CARTESIAN_POINT('Ctrl Pts',(6.12932483702202,-1.70493175725099,7.89868755123272));
#12515=CARTESIAN_POINT('Ctrl Pts',(6.13842358379824,-1.69937750447354,7.89936890451943));
#12516=CARTESIAN_POINT('Ctrl Pts',(6.14367293749366,-1.69613956889572,7.89976153193726));
#12517=CARTESIAN_POINT('Ctrl Pts',(6.15484709329693,-1.68917531360146,7.90059649649099));
#12518=CARTESIAN_POINT('Ctrl Pts',(6.16076749060382,-1.68544204087414,7.90103839491648));
#12519=CARTESIAN_POINT('Ctrl Pts',(6.17697301819635,-1.67510358171146,7.90224697853333));
#12520=CARTESIAN_POINT('Ctrl Pts',(6.18721745786905,-1.66843478513719,7.90300988275566));
#12521=CARTESIAN_POINT('Ctrl Pts',(6.21995579059073,-1.64669214219128,7.90544652243883));
#12522=CARTESIAN_POINT('Ctrl Pts',(6.24220513610413,-1.63125377295922,7.90710037292865));
#12523=CARTESIAN_POINT('Ctrl Pts',(6.33917146107056,-1.56100322148526,7.91433121135577));
#12524=CARTESIAN_POINT('Ctrl Pts',(6.41033540763591,-1.50147332450867,7.9197038438506));
#12525=CARTESIAN_POINT('Ctrl Pts',(6.57773991937719,-1.34035023714681,7.93319125840135));
#12526=CARTESIAN_POINT('Ctrl Pts',(6.66790995192704,-1.23320451905554,7.94130122088101));
#12527=CARTESIAN_POINT('Ctrl Pts',(6.75990306235257,-1.09718800246761,7.95140475770934));
#12528=CARTESIAN_POINT('Ctrl Pts',(6.77328161495573,-1.07659791797566,7.95292844054435));
#12529=CARTESIAN_POINT('Ctrl Pts',(6.79161112533453,-1.04721475944494,7.9550973864577));
#12530=CARTESIAN_POINT('Ctrl Pts',(6.79688100405623,-1.0386225221909,7.95573098361736));
#12531=CARTESIAN_POINT('Ctrl Pts',(6.80596326563009,-1.02355942823479,7.95684080628152));
#12532=CARTESIAN_POINT('Ctrl Pts',(6.80980467580243,-1.01710624324983,7.95731596791938));
#12533=CARTESIAN_POINT('Ctrl Pts',(6.81778513585097,-1.00352596878321,7.95831537078586));
#12534=CARTESIAN_POINT('Ctrl Pts',(6.82191663075262,-0.996394625749096,
7.95883987254407));
#12535=CARTESIAN_POINT('Ctrl Pts',(6.83168232875221,-0.979294682021079,
7.9600969236779));
#12536=CARTESIAN_POINT('Ctrl Pts',(6.8372750721431,-0.969302857917051,7.96083093701832));
#12537=CARTESIAN_POINT('Ctrl Pts',(6.85614227444794,-0.934903686414441,
7.96335657219048));
#12538=CARTESIAN_POINT('Ctrl Pts',(6.86899217847674,-0.910268363729511,
7.9651630344857));
#12539=CARTESIAN_POINT('Ctrl Pts',(6.89875827024245,-0.850173104793242,
7.96956636078178));
#12540=CARTESIAN_POINT('Ctrl Pts',(6.91514902314378,-0.814467279397957,
7.97218000464471));
#12541=CARTESIAN_POINT('Ctrl Pts',(6.98422589300265,-0.651458957983918,
7.98409941527029));
#12542=CARTESIAN_POINT('Ctrl Pts',(7.02468777710179,-0.519398848269831,
7.99375656232509));
#12543=CARTESIAN_POINT('Ctrl Pts',(7.06467948136437,-0.315676379723536,
8.00818527300753));
#12544=CARTESIAN_POINT('Ctrl Pts',(7.07452871502381,-0.24644146029606,8.01300296490859));
#12545=CARTESIAN_POINT('Ctrl Pts',(7.08287314268722,-0.152680442555139,
8.01930439382029));
#12546=CARTESIAN_POINT('Ctrl Pts',(7.08458189267994,-0.128494977962203,
8.02090984207486));
#12547=CARTESIAN_POINT('Ctrl Pts',(7.08626098899028,-0.0964207821697378,
8.02300737035582));
#12548=CARTESIAN_POINT('Ctrl Pts',(7.08662604207885,-0.0885559184528152,
8.02351918939281));
#12549=CARTESIAN_POINT('Ctrl Pts',(7.0871425850431,-0.075796664057269,8.02434522295565));
#12550=CARTESIAN_POINT('Ctrl Pts',(7.08732263218961,-0.0709036078754027,
8.02466097505791));
#12551=CARTESIAN_POINT('Ctrl Pts',(7.08762640566968,-0.0617289157230825,
8.02525104179397));
#12552=CARTESIAN_POINT('Ctrl Pts',(7.08775435916531,-0.0574475049421949,
8.02552558446984));
#12553=CARTESIAN_POINT('Ctrl Pts',(7.08798983547183,-0.0486156896671062,
8.02609029333832));
#12554=CARTESIAN_POINT('Ctrl Pts',(7.08809557651759,-0.044065240109889,
8.02638036173127));
#12555=CARTESIAN_POINT('Ctrl Pts',(7.08831313844747,-0.0330845257221766,
8.02707826876798));
#12556=CARTESIAN_POINT('Ctrl Pts',(7.08840944041291,-0.0266539558067715,
8.02748527688118));
#12557=CARTESIAN_POINT('Ctrl Pts',(7.0885412802017,-0.0136502073555671,
8.0283050782654));
#12558=CARTESIAN_POINT('Ctrl Pts',(7.08857543142776,-0.00707710677330047,
8.0287177952261));
#12559=CARTESIAN_POINT('Ctrl Pts',(7.08857709181481,-0.000503870024376882,
8.02912895344979));
#12560=CARTESIAN_POINT('Origin',(5.09382715545311,0.,-6.77268258743872));
#12561=CARTESIAN_POINT('',(7.08857715545311,-2.42987105381791E-11,8.98643389536848));
#12562=CARTESIAN_POINT('',(7.08857715545311,2.37118846529926E-11,8.82627928344061));
#12563=CARTESIAN_POINT('',(7.08857715545311,8.3550772080578E-14,-6.77268258743872));
#12564=CARTESIAN_POINT('Ctrl Pts',(7.08857715545311,-2.42987105381791E-11,
8.98643389536847));
#12565=CARTESIAN_POINT('Ctrl Pts',(7.08857715545217,-0.0768861299635129,
8.98188427170841));
#12566=CARTESIAN_POINT('Ctrl Pts',(7.08413199158264,-0.153700434669362,
8.97725037645284));
#12567=CARTESIAN_POINT('Ctrl Pts',(7.07351340805477,-0.245154605042594,
8.97153280431997));
#12568=CARTESIAN_POINT('Ctrl Pts',(7.07158860162889,-0.260226980213967,
8.97058406073964));
#12569=CARTESIAN_POINT('Ctrl Pts',(7.06812460096116,-0.28508826224742,8.96900782365654));
#12570=CARTESIAN_POINT('Ctrl Pts',(7.06668430181189,-0.294890479652502,
8.96838343332432));
#12571=CARTESIAN_POINT('Ctrl Pts',(7.06394499586537,-0.312614284625093,
8.96724898751005));
#12572=CARTESIAN_POINT('Ctrl Pts',(7.06267107287381,-0.320539579195344,
8.96673973220162));
#12573=CARTESIAN_POINT('Ctrl Pts',(7.05983097379962,-0.337552339224633,
8.96564218571651));
#12574=CARTESIAN_POINT('Ctrl Pts',(7.05824955293433,-0.346637036464673,
8.96505342371758));
#12575=CARTESIAN_POINT('Ctrl Pts',(7.053741860145,-0.371510086450372,8.96343393333251));
#12576=CARTESIAN_POINT('Ctrl Pts',(7.05068790132971,-0.387274308890986,
8.96239919267632));
#12577=CARTESIAN_POINT('Ctrl Pts',(7.03228433285138,-0.476489098409318,
8.95649455301054));
#12578=CARTESIAN_POINT('Ctrl Pts',(7.01299192665855,-0.549055805456616,
8.95150037752538));
#12579=CARTESIAN_POINT('Ctrl Pts',(6.95814209236811,-0.716679030325624,
8.9395123392995));
#12580=CARTESIAN_POINT('Ctrl Pts',(6.91933047072042,-0.810452754549243,
8.93244409452282));
#12581=CARTESIAN_POINT('Ctrl Pts',(6.84845799928886,-0.950467878084056,
8.92150726084807));
#12582=CARTESIAN_POINT('Ctrl Pts',(6.82128563742958,-0.999002620037872,
8.91764134562758));
#12583=CARTESIAN_POINT('Ctrl Pts',(6.76423917224009,-1.09159354332584,8.91018762972556));
#12584=CARTESIAN_POINT('Ctrl Pts',(6.73455768588789,-1.13571879224412,8.90659804740044));
#12585=CARTESIAN_POINT('Ctrl Pts',(6.69771101177791,-1.18603067177925,8.90250575321088));
#12586=CARTESIAN_POINT('Ctrl Pts',(6.69222450047737,-1.19341447708133,8.90190519378536));
#12587=CARTESIAN_POINT('Ctrl Pts',(6.6832335745464,-1.20534132506341,8.90093552576006));
#12588=CARTESIAN_POINT('Ctrl Pts',(6.67976036659062,-1.20990756950831,8.90056438021396));
#12589=CARTESIAN_POINT('Ctrl Pts',(6.67352589512187,-1.21803108808302,8.89990436535768));
#12590=CARTESIAN_POINT('Ctrl Pts',(6.67077224487407,-1.22159405119846,8.89961498199324));
#12591=CARTESIAN_POINT('Ctrl Pts',(6.66475168736986,-1.22932980134138,8.89898691034954));
#12592=CARTESIAN_POINT('Ctrl Pts',(6.66148021211496,-1.23349890188389,8.89864854921027));
#12593=CARTESIAN_POINT('Ctrl Pts',(6.65216926067984,-1.24526771183702,8.89769361584132));
#12594=CARTESIAN_POINT('Ctrl Pts',(6.646090772534,-1.25283656682012,8.89707972620055));
#12595=CARTESIAN_POINT('Ctrl Pts',(6.60630112023768,-1.3016479610396,8.89312019398319));
#12596=CARTESIAN_POINT('Ctrl Pts',(6.5710015160374,-1.34157441475001,8.88987856237572));
#12597=CARTESIAN_POINT('Ctrl Pts',(6.41543092826237,-1.50393940045418,8.87644751630348));
#12598=CARTESIAN_POINT('Ctrl Pts',(6.28122789122965,-1.61200392653529,8.8668121835552));
#12599=CARTESIAN_POINT('Ctrl Pts',(6.08222164566746,-1.7337558050609,8.85288298244007));
#12600=CARTESIAN_POINT('Ctrl Pts',(6.0281408006372,-1.76348795104782,8.84913668845719));
#12601=CARTESIAN_POINT('Ctrl Pts',(5.95872411697379,-1.79756105232033,8.8443280146994));
#12602=CARTESIAN_POINT('Ctrl Pts',(5.94459477265088,-1.80429125435264,8.8433493291224));
#12603=CARTESIAN_POINT('Ctrl Pts',(5.92201562471875,-1.81472214911176,8.84178481800752));
#12604=CARTESIAN_POINT('Ctrl Pts',(5.91361663478611,-1.81853177703217,8.84120273539858));
#12605=CARTESIAN_POINT('Ctrl Pts',(5.89785871807872,-1.82554792883914,8.84011029408799));
#12606=CARTESIAN_POINT('Ctrl Pts',(5.89050624404744,-1.82876855312802,8.83960042894666));
#12607=CARTESIAN_POINT('Ctrl Pts',(5.87403734417291,-1.83586430539414,8.83845795776896));
#12608=CARTESIAN_POINT('Ctrl Pts',(5.86491113754304,-1.83971605774887,8.83782457530857));
#12609=CARTESIAN_POINT('Ctrl Pts',(5.83791797043586,-1.85087249779595,8.83595013619377));
#12610=CARTESIAN_POINT('Ctrl Pts',(5.81997365093233,-1.85798583629272,8.83470270957932));
#12611=CARTESIAN_POINT('Ctrl Pts',(5.67579446958418,-1.91273248849412,8.8246661210579));
#12612=CARTESIAN_POINT('Ctrl Pts',(5.54514922678451,-1.94769798420551,8.81545195342419));
#12613=CARTESIAN_POINT('Ctrl Pts',(5.27710185000606,-1.99100742935538,8.79656440894279));
#12614=CARTESIAN_POINT('Ctrl Pts',(5.14031192627656,-1.99888591023311,8.78694140782125));
#12615=CARTESIAN_POINT('Ctrl Pts',(4.98855948659348,-1.99202874351317,8.77688607469454));
#12616=CARTESIAN_POINT('Ctrl Pts',(4.97334360153486,-1.99116637774985,8.7758851352434));
#12617=CARTESIAN_POINT('Ctrl Pts',(4.95224861962275,-1.98972810537196,8.77450892526519));
#12618=CARTESIAN_POINT('Ctrl Pts',(4.94636040498974,-1.98930037318386,8.77412602747462));
#12619=CARTESIAN_POINT('Ctrl Pts',(4.93623658102202,-1.98851976016467,8.77346993339159));
#12620=CARTESIAN_POINT('Ctrl Pts',(4.9320000817217,-1.9881794749837,8.77319605286148));
#12621=CARTESIAN_POINT('Ctrl Pts',(4.92313063702136,-1.98743852359684,8.77262411986344));
#12622=CARTESIAN_POINT('Ctrl Pts',(4.91849796176131,-1.98703519367603,8.77232622689462));
#12623=CARTESIAN_POINT('Ctrl Pts',(4.90716917715524,-1.98600895933872,8.77159971891355));
#12624=CARTESIAN_POINT('Ctrl Pts',(4.90047464752232,-1.98536837846942,8.77117207988868));
#12625=CARTESIAN_POINT('Ctrl Pts',(4.87629143783103,-1.98293087377884,8.76963293400567));
#12626=CARTESIAN_POINT('Ctrl Pts',(4.85882287030421,-1.9809365649555,8.76853183143856));
#12627=CARTESIAN_POINT('Ctrl Pts',(4.8152676773671,-1.97537977394779,8.7658080336922));
#12628=CARTESIAN_POINT('Ctrl Pts',(4.78922033401845,-1.97153124558076,8.76419856240537));
#12629=CARTESIAN_POINT('Ctrl Pts',(4.67637425800728,-1.95256809490912,8.75728106926091));
#12630=CARTESIAN_POINT('Ctrl Pts',(4.59054866339174,-1.93222727146068,8.75215976658576));
#12631=CARTESIAN_POINT('Ctrl Pts',(4.36699907829934,-1.86333292842259,8.73857743293405));
#12632=CARTESIAN_POINT('Ctrl Pts',(4.23280010509147,-1.80524654918499,8.73013619328223));
#12633=CARTESIAN_POINT('Ctrl Pts',(4.08454018405959,-1.72075134202396,8.71963392253941));
#12634=CARTESIAN_POINT('Ctrl Pts',(4.06317795220974,-1.70804200961265,8.71809097209041));
#12635=CARTESIAN_POINT('Ctrl Pts',(4.03367942197034,-1.68973714296457,8.71591571796825));
#12636=CARTESIAN_POINT('Ctrl Pts',(4.02533816647287,-1.68447502325769,8.71529554036448));
#12637=CARTESIAN_POINT('Ctrl Pts',(4.0101303712653,-1.67472270789988,8.71415529517673));
#12638=CARTESIAN_POINT('Ctrl Pts',(4.00325182098143,-1.67025156937388,8.71363593817461));
#12639=CARTESIAN_POINT('Ctrl Pts',(3.98936166952506,-1.66110042311804,8.71257971012247));
#12640=CARTESIAN_POINT('Ctrl Pts',(3.98235176873429,-1.6564181496325,8.71204276171826));
#12641=CARTESIAN_POINT('Ctrl Pts',(3.96509700138599,-1.64473395526746,8.71071126044905));
#12642=CARTESIAN_POINT('Ctrl Pts',(3.95488750244197,-1.63768067693914,8.70991478427794));
#12643=CARTESIAN_POINT('Ctrl Pts',(3.9167818972426,-1.61082658013847,8.7069089165668));
#12644=CARTESIAN_POINT('Ctrl Pts',(3.88933221577727,-1.59040545544929,8.70467602557586));
#12645=CARTESIAN_POINT('Ctrl Pts',(3.82155136846083,-1.53721855601956,8.69898560827842));
#12646=CARTESIAN_POINT('Ctrl Pts',(3.78195187679679,-1.50356545217721,8.69549548243061));
#12647=CARTESIAN_POINT('Ctrl Pts',(3.66016408295872,-1.39158879677805,8.68422825200392));
#12648=CARTESIAN_POINT('Ctrl Pts',(3.58332816119793,-1.30778376583525,8.67627827189778));
#12649=CARTESIAN_POINT('Ctrl Pts',(3.4582825948367,-1.14558354156204,8.66203591021737));
#12650=CARTESIAN_POINT('Ctrl Pts',(3.40754976563659,-1.06950462436886,8.65574428287472));
#12651=CARTESIAN_POINT('Ctrl Pts',(3.35676839910661,-0.980700968856299,
8.64902054810288));
#12652=CARTESIAN_POINT('Ctrl Pts',(3.35140988989883,-0.971148597775236,
8.64830499837596));
#12653=CARTESIAN_POINT('Ctrl Pts',(3.34341501250365,-0.956617279343384,
8.64722865227209));
#12654=CARTESIAN_POINT('Ctrl Pts',(3.3407207127681,-0.95167068454312,8.64686436951905));
#12655=CARTESIAN_POINT('Ctrl Pts',(3.33591310556014,-0.942754463339986,
8.64621163728329));
#12656=CARTESIAN_POINT('Ctrl Pts',(3.3337922461384,-0.938789062641845,8.64592272179111));
#12657=CARTESIAN_POINT('Ctrl Pts',(3.32916233090399,-0.930061605541731,
8.64528987742471));
#12658=CARTESIAN_POINT('Ctrl Pts',(3.32665913490921,-0.925296558897963,
8.64494631541515));
#12659=CARTESIAN_POINT('Ctrl Pts',(3.3195157286768,-0.911563751548811,8.6439616314221));
#12660=CARTESIAN_POINT('Ctrl Pts',(3.31492420005311,-0.902570660774414,
8.64332346315416));
#12661=CARTESIAN_POINT('Ctrl Pts',(3.28212997691631,-0.837116527885047,
8.63872402239285));
#12662=CARTESIAN_POINT('Ctrl Pts',(3.25654963249738,-0.779373958277573,
8.63490932965599));
#12663=CARTESIAN_POINT('Ctrl Pts',(3.186615409539,-0.598830701309576,8.62342646125249));
#12664=CARTESIAN_POINT('Ctrl Pts',(3.15153442409377,-0.472817656618723,
8.61600044493617));
#12665=CARTESIAN_POINT('Ctrl Pts',(3.11358467568438,-0.256235374654983,
8.60306763301469));
#12666=CARTESIAN_POINT('Ctrl Pts',(3.10409457636425,-0.167266817828607,
8.59771304159364));
#12667=CARTESIAN_POINT('Ctrl Pts',(3.09998889508395,-0.0623073507497877,
8.59119430501158));
#12668=CARTESIAN_POINT('Ctrl Pts',(3.09956089217759,-0.0466397237229232,
8.59021617096358));
#12669=CARTESIAN_POINT('Ctrl Pts',(3.09916148559782,-0.0209165895202022,
8.5886012323589));
#12670=CARTESIAN_POINT('Ctrl Pts',(3.09908140183857,-0.0108632739091539,
8.58796780616427));
#12671=CARTESIAN_POINT('Ctrl Pts',(3.09907405603421,0.00722851253278823,
8.58682364938202));
#12672=CARTESIAN_POINT('Ctrl Pts',(3.09911938218848,0.0152668016787727,
8.5863137829533));
#12673=CARTESIAN_POINT('Ctrl Pts',(3.09931982486487,0.0324225310801107,
8.5852222792427));
#12674=CARTESIAN_POINT('Ctrl Pts',(3.09948887677084,0.0415395948063888,
8.58464021939651));
#12675=CARTESIAN_POINT('Ctrl Pts',(3.10011622867037,0.0662361746737126,
8.58305793787235));
#12676=CARTESIAN_POINT('Ctrl Pts',(3.10069461928511,0.0818117405072412,
8.58205400624125));
#12677=CARTESIAN_POINT('Ctrl Pts',(3.10474190317115,0.164619422998105,8.57668336069927));
#12678=CARTESIAN_POINT('Ctrl Pts',(3.11142980511974,0.231643460043858,8.57221758295055));
#12679=CARTESIAN_POINT('Ctrl Pts',(3.1457476111784,0.458629711051173,8.55668432209717));
#12680=CARTESIAN_POINT('Ctrl Pts',(3.18948883210554,0.61550027988165,8.54518914496262));
#12681=CARTESIAN_POINT('Ctrl Pts',(3.27333552229397,0.817318324660651,8.53018373929405));
#12682=CARTESIAN_POINT('Ctrl Pts',(3.29713673405649,0.868391508567531,8.52637356877625));
#12683=CARTESIAN_POINT('Ctrl Pts',(3.32736643097465,0.926677482888834,8.52206371308));
#12684=CARTESIAN_POINT('Ctrl Pts',(3.33172110512173,0.934931507565759,8.52145432300223));
#12685=CARTESIAN_POINT('Ctrl Pts',(3.33886508750732,0.948245261303438,8.52047326905627));
#12686=CARTESIAN_POINT('Ctrl Pts',(3.34161867305235,0.95332385459402,8.52009949127387));
#12687=CARTESIAN_POINT('Ctrl Pts',(3.34655930266378,0.962342411996359,8.51943663660777));
#12688=CARTESIAN_POINT('Ctrl Pts',(3.34873767033393,0.966286995471901,8.51914702733419));
#12689=CARTESIAN_POINT('Ctrl Pts',(3.35349274696385,0.974828950386027,8.51852057661019));
#12690=CARTESIAN_POINT('Ctrl Pts',(3.35607431228292,0.979423500574573,8.51818404807517));
#12691=CARTESIAN_POINT('Ctrl Pts',(3.36339547555441,0.992333295091624,8.51723951827058));
#12692=CARTESIAN_POINT('Ctrl Pts',(3.36817682949126,1.00062486901939,8.51663410764764));
#12693=CARTESIAN_POINT('Ctrl Pts',(3.39849981598762,1.05234556997332,8.51286339713194));
#12694=CARTESIAN_POINT('Ctrl Pts',(3.42562181081653,1.09483234154442,8.50979100724284));
#12695=CARTESIAN_POINT('Ctrl Pts',(3.53780172510662,1.25669731365442,8.49800098503722));
#12696=CARTESIAN_POINT('Ctrl Pts',(3.63429958858564,1.36758477823499,8.48970510928694));
#12697=CARTESIAN_POINT('Ctrl Pts',(3.80615413487898,1.52594797700006,8.47594607970505));
#12698=CARTESIAN_POINT('Ctrl Pts',(3.87401953223029,1.58072314280811,8.47072084120669));
#12699=CARTESIAN_POINT('Ctrl Pts',(3.95799793978512,1.63986675163689,8.46434575294678));
#12700=CARTESIAN_POINT('Ctrl Pts',(3.97085822391302,1.64870001139537,8.46337202370236));
#12701=CARTESIAN_POINT('Ctrl Pts',(3.99215566579857,1.66296365820533,8.46176288177512));
#12702=CARTESIAN_POINT('Ctrl Pts',(4.00053267708518,1.66848295685161,8.46113080555867));
#12703=CARTESIAN_POINT('Ctrl Pts',(4.01569490016964,1.67830956289343,8.4599881113902));
#12704=CARTESIAN_POINT('Ctrl Pts',(4.02246522780034,1.68263952339214,8.45947834804337));
#12705=CARTESIAN_POINT('Ctrl Pts',(4.03698534055985,1.69180269473325,8.45838599819257));
#12706=CARTESIAN_POINT('Ctrl Pts',(4.04474250253744,1.69662381395242,8.45780298217343));
#12707=CARTESIAN_POINT('Ctrl Pts',(4.06588352603216,1.70956265721521,8.45621540346887));
#12708=CARTESIAN_POINT('Ctrl Pts',(4.07933005009587,1.71757625284766,8.45520708841639));
#12709=CARTESIAN_POINT('Ctrl Pts',(4.15198944460403,1.75972747058815,8.4497650795519));
#12710=CARTESIAN_POINT('Ctrl Pts',(4.21282678695162,1.79095939887924,8.44522913517843));
#12711=CARTESIAN_POINT('Ctrl Pts',(4.42955991635475,1.88850522519052,8.42913725373259));
#12712=CARTESIAN_POINT('Ctrl Pts',(4.5921760263042,1.93805016089112,8.41711100793078));
#12713=CARTESIAN_POINT('Ctrl Pts',(4.80717533295674,1.97464891138987,8.40220409720123));
#12714=CARTESIAN_POINT('Ctrl Pts',(4.85555772929438,1.98106944190795,8.39891807992833));
#12715=CARTESIAN_POINT('Ctrl Pts',(4.91306497354076,1.98656314802436,8.39512892916408));
#12716=CARTESIAN_POINT('Ctrl Pts',(4.92200484459242,1.98735633648343,8.39454321059797));
#12717=CARTESIAN_POINT('Ctrl Pts',(4.93660031035549,1.98855209195383,8.3935927093419));
#12718=CARTESIAN_POINT('Ctrl Pts',(4.94225269171582,1.98899092182216,8.39322601633843));
#12719=CARTESIAN_POINT('Ctrl Pts',(4.95239363218515,1.98973474604223,8.3925707476869));
#12720=CARTESIAN_POINT('Ctrl Pts',(4.95688140627286,1.99004865873386,8.39228168911091));
#12721=CARTESIAN_POINT('Ctrl Pts',(4.96671060636588,1.99070278798841,8.39165061663439));
#12722=CARTESIAN_POINT('Ctrl Pts',(4.97205234791763,1.99103669102747,8.39130895518265));
#12723=CARTESIAN_POINT('Ctrl Pts',(4.98733236623254,1.99193009474744,8.3903351834966));
#12724=CARTESIAN_POINT('Ctrl Pts',(4.99727374154781,1.99243672181617,8.38970592611087));
#12725=CARTESIAN_POINT('Ctrl Pts',(5.06634066297629,1.99543831261368,8.38536142173749));
#12726=CARTESIAN_POINT('Ctrl Pts',(5.12555395675346,1.99537576008364,8.38177487576219));
#12727=CARTESIAN_POINT('Ctrl Pts',(5.27756827611796,1.98844473611097,8.37272555693766));
#12728=CARTESIAN_POINT('Ctrl Pts',(5.37004859284434,1.97772006300377,8.3673684069124));
#12729=CARTESIAN_POINT('Ctrl Pts',(5.58923872019216,1.93662072453541,8.35440606374597));
#12730=CARTESIAN_POINT('Ctrl Pts',(5.71436354305339,1.90022647387958,8.34677012645167));
#12731=CARTESIAN_POINT('Ctrl Pts',(5.85011753619847,1.84589160690041,8.33770241937153));
#12732=CARTESIAN_POINT('Ctrl Pts',(5.86511060504782,1.83967735776198,8.33669014581121));
#12733=CARTESIAN_POINT('Ctrl Pts',(5.88942040117033,1.82925215297393,8.33503032597712));
#12734=CARTESIAN_POINT('Ctrl Pts',(5.89878371076913,1.82515122376565,8.33438649062051));
#12735=CARTESIAN_POINT('Ctrl Pts',(5.91546811112118,1.81769045306529,8.33323093185639));
#12736=CARTESIAN_POINT('Ctrl Pts',(5.92280119963922,1.81435786827327,8.33272014628719));
#12737=CARTESIAN_POINT('Ctrl Pts',(5.93023342020656,1.81092576880909,8.33219945699855));
#12738=CARTESIAN_POINT('Ctrl Pts',(5.93035301864395,1.81087052548448,8.33219107733513));
#12739=CARTESIAN_POINT('Ctrl Pts',(5.93063569325418,1.81073992219651,8.33217126987011));
#12740=CARTESIAN_POINT('Ctrl Pts',(5.93079876470571,1.81066455205763,8.33215984171894));
#12741=CARTESIAN_POINT('Ctrl Pts',(5.93111204402587,1.8105197058461,8.33213788407547));
#12742=CARTESIAN_POINT('Ctrl Pts',(5.93126225344108,1.81045023310424,8.33212735469762));
#12743=CARTESIAN_POINT('Ctrl Pts',(5.93155085113882,1.81031671136304,8.33210712217725));
#12744=CARTESIAN_POINT('Ctrl Pts',(5.93168924073376,1.81025266518316,8.33209741913152));
#12745=CARTESIAN_POINT('Ctrl Pts',(5.931955155254,1.81012956392626,8.33207877276479));
#12746=CARTESIAN_POINT('Ctrl Pts',(5.93208268128827,1.81007051123897,8.33206982952602));
#12747=CARTESIAN_POINT('Ctrl Pts',(5.93232774588016,1.80995699925015,8.33205264172367));
#12748=CARTESIAN_POINT('Ctrl Pts',(5.93244528538545,1.80990254197012,8.33204439722926));
#12749=CARTESIAN_POINT('Ctrl Pts',(5.93267118129554,1.80979785530666,8.33202855089063));
#12750=CARTESIAN_POINT('Ctrl Pts',(5.9327795384945,1.80974762764129,8.33202094910573));
#12751=CARTESIAN_POINT('Ctrl Pts',(5.93298780729639,1.80965106443957,8.33200633678234));
#12752=CARTESIAN_POINT('Ctrl Pts',(5.93308771958151,1.80960473035638,8.33199932629357));
#12753=CARTESIAN_POINT('Ctrl Pts',(5.93327977483871,1.80951564586344,8.33198584939493));
#12754=CARTESIAN_POINT('Ctrl Pts',(5.93337191838284,1.80947289668986,8.33197938302775));
#12755=CARTESIAN_POINT('Ctrl Pts',(5.93354905636797,1.8093906986619,8.33196695108956));
#12756=CARTESIAN_POINT('Ctrl Pts',(5.93363405129377,1.80935125085726,8.33196098555485));
#12757=CARTESIAN_POINT('Ctrl Pts',(5.93379746092356,1.8092753952625,8.33194951555891));
#12758=CARTESIAN_POINT('Ctrl Pts',(5.93387587605352,1.80923898835726,8.33194401112752));
#12759=CARTESIAN_POINT('Ctrl Pts',(5.93402664810861,1.80916897536033,8.33193342686913));
#12760=CARTESIAN_POINT('Ctrl Pts',(5.93409900537906,1.80913537002816,8.33192834706865));
#12761=CARTESIAN_POINT('Ctrl Pts',(5.93423814080111,1.80907074036043,8.33191857858641));
#12762=CARTESIAN_POINT('Ctrl Pts',(5.93430491924985,1.80903971666878,8.33191388992694));
#12763=CARTESIAN_POINT('Ctrl Pts',(5.93443333686407,1.80898004822983,8.33190487297095));
#12764=CARTESIAN_POINT('Ctrl Pts',(5.93449497629299,1.80895140402506,8.33190054469265));
#12765=CARTESIAN_POINT('Ctrl Pts',(5.93461351986193,1.80889630876453,8.33189222023801));
#12766=CARTESIAN_POINT('Ctrl Pts',(5.93467042421093,1.80886985817731,8.33188822407822));
#12767=CARTESIAN_POINT('Ctrl Pts',(5.93481394540416,1.80880313764433,8.33187814471686));
#12768=CARTESIAN_POINT('Ctrl Pts',(5.93490056058505,1.80876286417095,8.33187206139461));
#12769=CARTESIAN_POINT('Ctrl Pts',(5.93507230327991,1.8086829939413,8.3318599984062));
#12770=CARTESIAN_POINT('Ctrl Pts',(5.93515743090216,1.80864339739138,8.33185401874661));
#12771=CARTESIAN_POINT('Ctrl Pts',(5.93532623282861,1.8085648657965,8.33184216071285));
#12772=CARTESIAN_POINT('Ctrl Pts',(5.9354099072215,1.80852593095683,8.33183628234607));
#12773=CARTESIAN_POINT('Ctrl Pts',(5.94418633816392,1.80444139660216,8.33121967189457));
#12774=CARTESIAN_POINT('Ctrl Pts',(5.95284968817242,1.80033324037226,8.33060679308141));
#12775=CARTESIAN_POINT('Ctrl Pts',(5.97771805022388,1.78832031026126,8.3288351479526));
#12776=CARTESIAN_POINT('Ctrl Pts',(5.99384560396007,1.78025824054228,8.32767096904429));
#12777=CARTESIAN_POINT('Ctrl Pts',(6.03011286853432,1.76150968173623,8.32501754142283));
#12778=CARTESIAN_POINT('Ctrl Pts',(6.05018282345811,1.75069445117057,8.32352394320666));
#12779=CARTESIAN_POINT('Ctrl Pts',(6.114781433277,1.71444147054619,8.31863284198301));
#12780=CARTESIAN_POINT('Ctrl Pts',(6.15851275476344,1.68763178540857,8.31518950509405));
#12781=CARTESIAN_POINT('Ctrl Pts',(6.29920847943317,1.59373117748438,8.30367584203508));
#12782=CARTESIAN_POINT('Ctrl Pts',(6.39125794563229,1.51973436816758,8.29541147782027));
#12783=CARTESIAN_POINT('Ctrl Pts',(6.53971008470285,1.37702734462932,8.28110151323893));
#12784=CARTESIAN_POINT('Ctrl Pts',(6.59908988729707,1.31185726720574,8.27504433863938));
#12785=CARTESIAN_POINT('Ctrl Pts',(6.66079155827713,1.23441073021474,8.26853612773482));
#12786=CARTESIAN_POINT('Ctrl Pts',(6.66753941210539,1.22579649076068,8.26782125243606));
#12787=CARTESIAN_POINT('Ctrl Pts',(6.67765174048795,1.212666049915,8.26674571656514));
#12788=CARTESIAN_POINT('Ctrl Pts',(6.68106841005942,1.20819057533575,8.26638157724237));
#12789=CARTESIAN_POINT('Ctrl Pts',(6.68717968426723,1.20011478743902,8.2657289951711));
#12790=CARTESIAN_POINT('Ctrl Pts',(6.68988109269775,1.19651979285541,8.26544008742162));
#12791=CARTESIAN_POINT('Ctrl Pts',(6.69579035901357,1.18860020505537,8.26480713413915));
#12792=CARTESIAN_POINT('Ctrl Pts',(6.69899286984829,1.18427175259263,8.26446345634563));
#12793=CARTESIAN_POINT('Ctrl Pts',(6.70815560169035,1.17178212849741,8.26347810598919));
#12794=CARTESIAN_POINT('Ctrl Pts',(6.71407148439505,1.16358842107007,8.26283939335486));
#12795=CARTESIAN_POINT('Ctrl Pts',(6.75662710421767,1.10369349163699,8.25822346757823));
#12796=CARTESIAN_POINT('Ctrl Pts',(6.79085100798916,1.05031174920634,8.25439403239074));
#12797=CARTESIAN_POINT('Ctrl Pts',(6.89077320284531,0.876780394944098,8.2425200051691));
#12798=CARTESIAN_POINT('Ctrl Pts',(6.9466819209477,0.751459313874922,8.23474557418199));
#12799=CARTESIAN_POINT('Ctrl Pts',(7.00605985454118,0.570334326301552,8.2235022825315));
#12800=CARTESIAN_POINT('Ctrl Pts',(7.02072836183434,0.518619576807721,8.22029487172644));
#12801=CARTESIAN_POINT('Ctrl Pts',(7.04192616888963,0.430467162853203,8.21478072001062));
#12802=CARTESIAN_POINT('Ctrl Pts',(7.04956212233093,0.394325014991496,8.21250715945146));
#12803=CARTESIAN_POINT('Ctrl Pts',(7.05855933338069,0.345006247997024,8.20937792601514));
#12804=CARTESIAN_POINT('Ctrl Pts',(7.06079954723259,0.331996142844514,8.20854996035052));
#12805=CARTESIAN_POINT('Ctrl Pts',(7.0641477185964,0.311326702201238,8.20723022730679));
#12806=CARTESIAN_POINT('Ctrl Pts',(7.06534055094648,0.303681355556016,8.20674114115148));
#12807=CARTESIAN_POINT('Ctrl Pts',(7.06764215524666,0.288344069974504,8.20575803004754));
#12808=CARTESIAN_POINT('Ctrl Pts',(7.068750518875,0.280652208109691,8.20526400152734));
#12809=CARTESIAN_POINT('Ctrl Pts',(7.07088754613947,0.265181707018643,8.20426831591472));
#12810=CARTESIAN_POINT('Ctrl Pts',(7.07191531690994,0.257403086162201,8.20376664015122));
#12811=CARTESIAN_POINT('Ctrl Pts',(7.07416351492177,0.23957853480187,8.20261459723933));
#12812=CARTESIAN_POINT('Ctrl Pts',(7.07535343194504,0.229529040219516,8.20196328603193));
#12813=CARTESIAN_POINT('Ctrl Pts',(7.0793888932144,0.193073824154529,8.1995939081006));
#12814=CARTESIAN_POINT('Ctrl Pts',(7.0817833742856,0.16662195568988,8.19786191458116));
#12815=CARTESIAN_POINT('Ctrl Pts',(7.08696839553794,0.0929961691002093,
8.19300382847231));
#12816=CARTESIAN_POINT('Ctrl Pts',(7.08861171175909,0.04576206065972,8.18984437323121));
#12817=CARTESIAN_POINT('Ctrl Pts',(7.08857660471244,-0.00148228863371718,
8.18664306094147));
#12818=CARTESIAN_POINT('Ctrl Pts',(7.0885770914503,-0.000505311004862244,
8.02912886331594));
#12819=CARTESIAN_POINT('Ctrl Pts',(7.08858251806087,0.0209166073635135,
8.03046881243805));
#12820=CARTESIAN_POINT('Ctrl Pts',(7.08824286466212,0.0423383398002704,
8.03179210744699));
#12821=CARTESIAN_POINT('Ctrl Pts',(7.08330683993958,0.196704910921732,8.0412343602088));
#12822=CARTESIAN_POINT('Ctrl Pts',(7.06576668731101,0.328914167340696,8.04883839769366));
#12823=CARTESIAN_POINT('Ctrl Pts',(7.01596266478146,0.539836700377552,8.06144819132248));
#12824=CARTESIAN_POINT('Ctrl Pts',(6.99163096249784,0.619973938727455,8.06635430442614));
#12825=CARTESIAN_POINT('Ctrl Pts',(6.94571488809877,0.74282900711577,8.07426859149292));
#12826=CARTESIAN_POINT('Ctrl Pts',(6.9275058841988,0.786705079275837,8.07717666730591));
#12827=CARTESIAN_POINT('Ctrl Pts',(6.9019385443612,0.842588789713423,8.08100819488785));
#12828=CARTESIAN_POINT('Ctrl Pts',(6.89599429150016,0.855228777198025,8.08188344848281));
#12829=CARTESIAN_POINT('Ctrl Pts',(6.88610530183051,0.875695958024054,8.08331527850948));
#12830=CARTESIAN_POINT('Ctrl Pts',(6.88224079348846,0.883561554285801,8.08386907968198));
#12831=CARTESIAN_POINT('Ctrl Pts',(6.87469654244288,0.89866440020061,8.08493941293801));
#12832=CARTESIAN_POINT('Ctrl Pts',(6.87102419258478,0.905905163761391,8.08545567944673));
#12833=CARTESIAN_POINT('Ctrl Pts',(6.86248507869253,0.922489949639226,8.08664545760591));
#12834=CARTESIAN_POINT('Ctrl Pts',(6.85758831892418,0.931818173161683,8.08732001118322));
#12835=CARTESIAN_POINT('Ctrl Pts',(6.84169684231514,0.961517009108036,8.08948507979792));
#12836=CARTESIAN_POINT('Ctrl Pts',(6.83042166863756,0.981734599214327,8.09098544697355));
#12837=CARTESIAN_POINT('Ctrl Pts',(6.73435337694826,1.14715994975751,8.10348761656134));
#12838=CARTESIAN_POINT('Ctrl Pts',(6.63187659969673,1.28128216831225,8.11516608799867));
#12839=CARTESIAN_POINT('Ctrl Pts',(6.44166860061383,1.47407863303438,8.13403576160537));
#12840=CARTESIAN_POINT('Ctrl Pts',(6.36395670642084,1.54154471052709,8.14115701217674));
#12841=CARTESIAN_POINT('Ctrl Pts',(6.27461501859275,1.60774331296646,8.14847679566218));
#12842=CARTESIAN_POINT('Ctrl Pts',(6.26781415209506,1.61271605548102,8.14902887121365));
#12843=CARTESIAN_POINT('Ctrl Pts',(6.25517826253906,1.62183303217412,8.15004488410969));
#12844=CARTESIAN_POINT('Ctrl Pts',(6.24935207736232,1.62598921791927,8.15050956960234));
#12845=CARTESIAN_POINT('Ctrl Pts',(6.23967638133744,1.63281323086345,8.15127488453989));
#12846=CARTESIAN_POINT('Ctrl Pts',(6.23583967614752,1.63549897554897,8.15157670467607));
#12847=CARTESIAN_POINT('Ctrl Pts',(6.22829969410445,1.64073759390073,8.15216656417929));
#12848=CARTESIAN_POINT('Ctrl Pts',(6.22459719063908,1.64329149002111,8.15245466978984));
#12849=CARTESIAN_POINT('Ctrl Pts',(6.21533551155887,1.64963384592458,8.1531715939762));
#12850=CARTESIAN_POINT('Ctrl Pts',(6.20976568609022,1.65340679126196,8.15359937726235));
#12851=CARTESIAN_POINT('Ctrl Pts',(6.19069794281657,1.66618284765166,8.15505280548452));
#12852=CARTESIAN_POINT('Ctrl Pts',(6.17710890987038,1.67504969654972,8.15606985649493));
#12853=CARTESIAN_POINT('Ctrl Pts',(6.07906264973981,1.73733261114568,8.16328620545652));
#12854=CARTESIAN_POINT('Ctrl Pts',(5.99079426573619,1.78450793293673,8.16914672343449));
#12855=CARTESIAN_POINT('Ctrl Pts',(5.81221707027307,1.86333445751262,8.18050455438396));
#12856=CARTESIAN_POINT('Ctrl Pts',(5.72244224080311,1.89550569494378,8.18599300302687));
#12857=CARTESIAN_POINT('Ctrl Pts',(5.57977520500691,1.93537579453606,8.19474985383873));
#12858=CARTESIAN_POINT('Ctrl Pts',(5.52829355516862,1.94757883349386,8.1979150992948));
#12859=CARTESIAN_POINT('Ctrl Pts',(5.44237684918372,1.96436803506055,8.20325307012839));
#12860=CARTESIAN_POINT('Ctrl Pts',(5.40819751425057,1.97012682866522,8.20539072435081));
#12861=CARTESIAN_POINT('Ctrl Pts',(5.36154047116294,1.97674293871183,8.20833555284953));
#12862=CARTESIAN_POINT('Ctrl Pts',(5.34917799885267,1.97837787106688,8.20911835234385));
#12863=CARTESIAN_POINT('Ctrl Pts',(5.32842157975269,1.98092511080476,8.21043723105269));
#12864=CARTESIAN_POINT('Ctrl Pts',(5.3200355931394,1.98190024413456,8.21097132986456));
#12865=CARTESIAN_POINT('Ctrl Pts',(5.30349844810045,1.98371687961533,8.21202713495702));
#12866=CARTESIAN_POINT('Ctrl Pts',(5.29534778931679,1.9845614478462,8.21254873406146));
#12867=CARTESIAN_POINT('Ctrl Pts',(5.27741423704017,1.98630809860511,8.21369917510282));
#12868=CARTESIAN_POINT('Ctrl Pts',(5.26762946308296,1.98718817208549,8.21432869239916));
#12869=CARTESIAN_POINT('Ctrl Pts',(5.23330664651686,1.99001983744563,8.21654350929019));
#12870=CARTESIAN_POINT('Ctrl Pts',(5.20874015941342,1.99158941396377,8.21814062510251));
#12871=CARTESIAN_POINT('Ctrl Pts',(5.03347179218353,1.99953392188722,8.22962441370651));
#12872=CARTESIAN_POINT('Ctrl Pts',(4.88252998948568,1.98925010129459,8.24003944089881));
#12873=CARTESIAN_POINT('Ctrl Pts',(4.65111298145257,1.94683600092371,8.25644212576776));
#12874=CARTESIAN_POINT('Ctrl Pts',(4.56905355768173,1.92633862831664,8.26233441767993));
#12875=CARTESIAN_POINT('Ctrl Pts',(4.4640415149418,1.89289685946804,8.26980782260311));
#12876=CARTESIAN_POINT('Ctrl Pts',(4.43969733495707,1.8846227155951,8.27153512329383));
#12877=CARTESIAN_POINT('Ctrl Pts',(4.39927672673215,1.87000683459093,8.27438690642788));
#12878=CARTESIAN_POINT('Ctrl Pts',(4.38311096679276,1.86392285433591,8.2755230362087));
#12879=CARTESIAN_POINT('Ctrl Pts',(4.36080654584855,1.85519620148584,8.27708248246566));
#12880=CARTESIAN_POINT('Ctrl Pts',(4.35459961242113,1.85273171366393,8.27751557028158));
#12881=CARTESIAN_POINT('Ctrl Pts',(4.34410031590908,1.84850176284116,8.27824652226261));
#12882=CARTESIAN_POINT('Ctrl Pts',(4.33980155653575,1.84675241950539,8.27854533085519));
#12883=CARTESIAN_POINT('Ctrl Pts',(4.33156848127149,1.84336849968653,8.27911666697057));
#12884=CARTESIAN_POINT('Ctrl Pts',(4.32763326095993,1.84173630818035,8.27938933969216));
#12885=CARTESIAN_POINT('Ctrl Pts',(4.31822181810818,1.83779738608704,8.28004054153849));
#12886=CARTESIAN_POINT('Ctrl Pts',(4.31275057601281,1.83547875248459,8.28041836232799));
#12887=CARTESIAN_POINT('Ctrl Pts',(4.29304373435961,1.82702320308407,8.28177681217749));
#12888=CARTESIAN_POINT('Ctrl Pts',(4.27886899855799,1.82074465787578,8.2827493437851));
#12889=CARTESIAN_POINT('Ctrl Pts',(4.14549696155639,1.75979929171473,8.2918697894921));
#12890=CARTESIAN_POINT('Ctrl Pts',(4.03187295569726,1.69366075541644,8.29942367317559));
#12891=CARTESIAN_POINT('Ctrl Pts',(3.8107025879474,1.53385013738658,8.31526532361536));
#12892=CARTESIAN_POINT('Ctrl Pts',(3.70503759851615,1.43887503210483,8.32353472504687));
#12893=CARTESIAN_POINT('Ctrl Pts',(3.59808696493624,1.31989553804707,8.33345220169072));
#12894=CARTESIAN_POINT('Ctrl Pts',(3.58603259641644,1.30610814325686,8.33459488664062));
#12895=CARTESIAN_POINT('Ctrl Pts',(3.56788516642986,1.28476563703569,8.33635491566129));
#12896=CARTESIAN_POINT('Ctrl Pts',(3.56165436066719,1.27732854722181,8.3369666209017));
#12897=CARTESIAN_POINT('Ctrl Pts',(3.55087125813924,1.26426541212841,8.33803844961714));
#12898=CARTESIAN_POINT('Ctrl Pts',(3.54629482636944,1.25865945416265,8.33849758696586));
#12899=CARTESIAN_POINT('Ctrl Pts',(3.53603263773524,1.24594807945994,8.33953687657863));
#12900=CARTESIAN_POINT('Ctrl Pts',(3.53036482625584,1.23882844527107,8.34011773177511));
#12901=CARTESIAN_POINT('Ctrl Pts',(3.51517434557535,1.21947659805728,8.34169334400111));
#12902=CARTESIAN_POINT('Ctrl Pts',(3.5057453833678,1.20717195547585,8.34269175787554));
#12903=CARTESIAN_POINT('Ctrl Pts',(3.46199922717546,1.14868431728759,8.34742258294061));
#12904=CARTESIAN_POINT('Ctrl Pts',(3.42955024247315,1.10114454163414,8.3512257396862));
#12905=CARTESIAN_POINT('Ctrl Pts',(3.29940960558362,0.891560654485373,8.36782518059771));
#12906=CARTESIAN_POINT('Ctrl Pts',(3.22300188684097,0.717502778069679,8.38131809175999));
#12907=CARTESIAN_POINT('Ctrl Pts',(3.16106719270336,0.495178833552528,8.39700661807852));
#12908=CARTESIAN_POINT('Ctrl Pts',(3.15114624964832,0.454702781591051,8.39979839589397));
#12909=CARTESIAN_POINT('Ctrl Pts',(3.14061470556361,0.405057025541294,8.40312145803544));
#12910=CARTESIAN_POINT('Ctrl Pts',(3.13879045134856,0.396158505502843,8.40371315699248));
#12911=CARTESIAN_POINT('Ctrl Pts',(3.13602449843945,0.38218187505547,8.40463603947316));
#12912=CARTESIAN_POINT('Ctrl Pts',(3.13504165414558,0.377112172649173,8.40496946038762));
#12913=CARTESIAN_POINT('Ctrl Pts',(3.13323508122034,0.367595879247602,8.40559274929203));
#12914=CARTESIAN_POINT('Ctrl Pts',(3.13240679281982,0.363150345583298,8.40588285860311));
#12915=CARTESIAN_POINT('Ctrl Pts',(3.13054357121205,0.352957826505537,8.40654562688854));
#12916=CARTESIAN_POINT('Ctrl Pts',(3.12951874948858,0.3472090836459,8.40691771409429));
#12917=CARTESIAN_POINT('Ctrl Pts',(3.12684963772621,0.331846550350842,8.40790765194156));
#12918=CARTESIAN_POINT('Ctrl Pts',(3.12525056381405,0.322224921536757,8.40852305987001));
#12919=CARTESIAN_POINT('Ctrl Pts',(3.11286504184186,0.244165338931582,8.41348145969738));
#12920=CARTESIAN_POINT('Ctrl Pts',(3.10557902584076,0.175211731448138,8.4176483792396));
#12921=CARTESIAN_POINT('Ctrl Pts',(3.09389006622732,-0.044420719629715,
8.43063610357305));
#12922=CARTESIAN_POINT('Ctrl Pts',(3.1029500579936,-0.195274428597169,8.43917042205476));
#12923=CARTESIAN_POINT('Ctrl Pts',(3.14017136784546,-0.408083455549092,
8.45204781741629));
#12924=CARTESIAN_POINT('Ctrl Pts',(3.15459595434313,-0.471894133822141,
8.45601468193832));
#12925=CARTESIAN_POINT('Ctrl Pts',(3.17627076682403,-0.549767178981537,
8.4610438783365));
#12926=CARTESIAN_POINT('Ctrl Pts',(3.18058803950855,-0.564608287914711,
8.46201086084256));
#12927=CARTESIAN_POINT('Ctrl Pts',(3.18771760357172,-0.588095715646715,
8.46355541786468));
#12928=CARTESIAN_POINT('Ctrl Pts',(3.19041734980186,-0.596775755101909,
8.46412933238892));
#12929=CARTESIAN_POINT('Ctrl Pts',(3.19561727315955,-0.613099897900092,
8.46521466776373));
#12930=CARTESIAN_POINT('Ctrl Pts',(3.19810454222504,-0.620747946146378,
8.4657256576209));
#12931=CARTESIAN_POINT('Ctrl Pts',(3.20381870828088,-0.637963621633583,
8.46688163301552));
#12932=CARTESIAN_POINT('Ctrl Pts',(3.20707211865166,-0.647522152393601,
8.46752747845391));
#12933=CARTESIAN_POINT('Ctrl Pts',(3.2156076472777,-0.671988983575927,8.46919117625997));
#12934=CARTESIAN_POINT('Ctrl Pts',(3.22099468293552,-0.686859680722899,
8.47021246033649));
#12935=CARTESIAN_POINT('Ctrl Pts',(3.25950708254536,-0.789348878406707,
8.47732290018869));
#12936=CARTESIAN_POINT('Ctrl Pts',(3.29858669607508,-0.874590745668232,
8.48361021640595));
#12937=CARTESIAN_POINT('Ctrl Pts',(3.42555110413713,-1.10686239746261,8.50178190473632));
#12938=CARTESIAN_POINT('Ctrl Pts',(3.52655988983565,-1.24577718849533,8.51397567667169));
#12939=CARTESIAN_POINT('Ctrl Pts',(3.65469063042048,-1.3813593433869,8.52644061005131));
#12940=CARTESIAN_POINT('Ctrl Pts',(3.66546272227107,-1.39249511725272,8.52746852702062));
#12941=CARTESIAN_POINT('Ctrl Pts',(3.68460581394031,-1.41182859874492,8.52925873141401));
#12942=CARTESIAN_POINT('Ctrl Pts',(3.69292121725599,-1.4200800504525,8.53002461864009));
#12943=CARTESIAN_POINT('Ctrl Pts',(3.70539967897826,-1.43224625829029,8.53115595780354));
#12944=CARTESIAN_POINT('Ctrl Pts',(3.709507471702,-1.43621698115368,8.53152553348375));
#12945=CARTESIAN_POINT('Ctrl Pts',(3.71688222903986,-1.44328462004672,8.5321838664326));
#12946=CARTESIAN_POINT('Ctrl Pts',(3.72014266241019,-1.44638817048052,8.53247312679796));
#12947=CARTESIAN_POINT('Ctrl Pts',(3.7272775953262,-1.45313390213895,8.53310221813287));
#12948=CARTESIAN_POINT('Ctrl Pts',(3.73115615851254,-1.45677163395887,8.53344171322459));
#12949=CARTESIAN_POINT('Ctrl Pts',(3.74202044743837,-1.46687997242698,8.53438593925357));
#12950=CARTESIAN_POINT('Ctrl Pts',(3.7490381352246,-1.47331623520628,8.53498814091406));
#12951=CARTESIAN_POINT('Ctrl Pts',(3.78828009745533,-1.50879294763232,8.53831480908532));
#12952=CARTESIAN_POINT('Ctrl Pts',(3.82140147678086,-1.53682881083467,8.54097140728786));
#12953=CARTESIAN_POINT('Ctrl Pts',(3.96971141029772,-1.65428196234825,8.55235858167986));
#12954=CARTESIAN_POINT('Ctrl Pts',(4.09359596654081,-1.73200151596034,8.56061703646805));
#12955=CARTESIAN_POINT('Ctrl Pts',(4.3030957794994,-1.8333922186254,8.57427776584483));
#12956=CARTESIAN_POINT('Ctrl Pts',(4.38372018901782,-1.86609985613317,8.57946462700225));
#12957=CARTESIAN_POINT('Ctrl Pts',(4.48726042658427,-1.90041994320643,8.58619684775099));
#12958=CARTESIAN_POINT('Ctrl Pts',(4.50842048798065,-1.90704434398851,8.58757592840611));
#12959=CARTESIAN_POINT('Ctrl Pts',(4.53972688898628,-1.91627504365491,8.58962298865096));
#12960=CARTESIAN_POINT('Ctrl Pts',(4.54979083388597,-1.9191564872006,8.59028205475521));
#12961=CARTESIAN_POINT('Ctrl Pts',(4.56766595928698,-1.92412247820514,8.59145464018497));
#12962=CARTESIAN_POINT('Ctrl Pts',(4.57546806454906,-1.92623902079519,8.5919671135139));
#12963=CARTESIAN_POINT('Ctrl Pts',(4.59186602792484,-1.93058059309345,8.5930456877877));
#12964=CARTESIAN_POINT('Ctrl Pts',(4.60046428951419,-1.93279576735484,8.59361209333547));
#12965=CARTESIAN_POINT('Ctrl Pts',(4.62313632437615,-1.93847563208265,8.59510799045172));
#12966=CARTESIAN_POINT('Ctrl Pts',(4.63723336170456,-1.94184441287745,8.5960405289032));
#12967=CARTESIAN_POINT('Ctrl Pts',(4.69761572769017,-1.95558017893758,8.60004600109448));
#12968=CARTESIAN_POINT('Ctrl Pts',(4.74422288914394,-1.9644473935644,8.60316595430959));
#12969=CARTESIAN_POINT('Ctrl Pts',(4.97595077612397,-2.00002714378665,8.61882681360413));
#12970=CARTESIAN_POINT('Ctrl Pts',(5.16386607788232,-2.00226797880707,8.63211021460256));
#12971=CARTESIAN_POINT('Ctrl Pts',(5.40345533786732,-1.97132972157052,8.6486738400749));
#12972=CARTESIAN_POINT('Ctrl Pts',(5.45731716406399,-1.96211280652047,8.65236285635033));
#12973=CARTESIAN_POINT('Ctrl Pts',(5.52028894483963,-1.94865422822784,8.65658499714032));
#12974=CARTESIAN_POINT('Ctrl Pts',(5.52982546226143,-1.94654269019723,8.65722190359077));
#12975=CARTESIAN_POINT('Ctrl Pts',(5.54452432165419,-1.94317468239781,8.65819931608898));
#12976=CARTESIAN_POINT('Ctrl Pts',(5.54969764123958,-1.94196752900474,8.65854250132478));
#12977=CARTESIAN_POINT('Ctrl Pts',(5.55924613021899,-1.93969920536832,8.6591743320978));
#12978=CARTESIAN_POINT('Ctrl Pts',(5.56362250992979,-1.9386438958638,8.65946329225351));
#12979=CARTESIAN_POINT('Ctrl Pts',(5.57355140504399,-1.93621406991845,8.66011747081952));
#12980=CARTESIAN_POINT('Ctrl Pts',(5.57910159957395,-1.93483048250477,8.66048216704427));
#12981=CARTESIAN_POINT('Ctrl Pts',(5.59350704671697,-1.93117351625073,8.66142634956856));
#12982=CARTESIAN_POINT('Ctrl Pts',(5.60235287334175,-1.92886307064639,8.66200379202124));
#12983=CARTESIAN_POINT('Ctrl Pts',(5.6615950072679,-1.91295371366528,8.66585720895393));
#12984=CARTESIAN_POINT('Ctrl Pts',(5.71146137050406,-1.89744070967401,8.66903366645225));
#12985=CARTESIAN_POINT('Ctrl Pts',(5.91719165158419,-1.82446738501356,8.68207493178618));
#12986=CARTESIAN_POINT('Ctrl Pts',(6.06617514596389,-1.74961603315116,8.69141659753913));
#12987=CARTESIAN_POINT('Ctrl Pts',(6.26056670204711,-1.61936892377206,8.70534274481421));
#12988=CARTESIAN_POINT('Ctrl Pts',(6.31499731187939,-1.57872697835795,8.70945640249277));
#12989=CARTESIAN_POINT('Ctrl Pts',(6.37927239960398,-1.52541869155086,8.71465064829089));
#12990=CARTESIAN_POINT('Ctrl Pts',(6.39118029638218,-1.51530408373663,8.71562794480809));
#12991=CARTESIAN_POINT('Ctrl Pts',(6.40985415136407,-1.49906097535857,8.71718518080149));
#12992=CARTESIAN_POINT('Ctrl Pts',(6.41669912642473,-1.49302398030502,8.71776135456346));
#12993=CARTESIAN_POINT('Ctrl Pts',(6.42949361859769,-1.4815826879341,8.7188486090298));
#12994=CARTESIAN_POINT('Ctrl Pts',(6.4354523883057,-1.47618897619571,8.71935924124324));
#12995=CARTESIAN_POINT('Ctrl Pts',(6.44878199469795,-1.46397601604263,8.72051125705207));
#12996=CARTESIAN_POINT('Ctrl Pts',(6.4561342209239,-1.45713686565038,8.72115347627051));
#12997=CARTESIAN_POINT('Ctrl Pts',(6.47480005068658,-1.43950888017823,8.72280163659338));
#12998=CARTESIAN_POINT('Ctrl Pts',(6.48603886253647,-1.42864218513244,8.72381090200112));
#12999=CARTESIAN_POINT('Ctrl Pts',(6.55983867822185,-1.35558801711397,8.73055314346655));
#13000=CARTESIAN_POINT('Ctrl Pts',(6.61833478770932,-1.28945001544624,8.73646092925677));
#13001=CARTESIAN_POINT('Ctrl Pts',(6.75268843812737,-1.11557645449979,8.75150759052761));
#13002=CARTESIAN_POINT('Ctrl Pts',(6.82262043869341,-1.00379381895217,8.76078608390787));
#13003=CARTESIAN_POINT('Ctrl Pts',(6.90915760239952,-0.829223211579989,
8.77420670870219));
#13004=CARTESIAN_POINT('Ctrl Pts',(6.93456292949947,-0.771186928061262,
8.77850413407092));
#13005=CARTESIAN_POINT('Ctrl Pts',(6.96077324167648,-0.702596584522218,
8.7833216827151));
#13006=CARTESIAN_POINT('Ctrl Pts',(6.96430817035543,-0.693130891392002,
8.78398086589617));
#13007=CARTESIAN_POINT('Ctrl Pts',(6.96961626501422,-0.678580698977294,
8.7849850454084));
#13008=CARTESIAN_POINT('Ctrl Pts',(6.97144096157011,-0.673515363819161,
8.78533295092669));
#13009=CARTESIAN_POINT('Ctrl Pts',(6.97475206710415,-0.664205737172418,
8.78596921390301));
#13010=CARTESIAN_POINT('Ctrl Pts',(6.9762446304581,-0.659963813517728,8.78625792051927));
#13011=CARTESIAN_POINT('Ctrl Pts',(6.97957390264843,-0.650398705194746,
8.78690623266583));
#13012=CARTESIAN_POINT('Ctrl Pts',(6.981402421407,-0.645072776902345,8.78726535634368));
#13013=CARTESIAN_POINT('Ctrl Pts',(6.98671835523619,-0.629372899194462,
8.78831871395971));
#13014=CARTESIAN_POINT('Ctrl Pts',(6.99014304260979,-0.618977713080454,
8.7890094034956));
#13015=CARTESIAN_POINT('Ctrl Pts',(7.02046019823809,-0.524340132543225,
8.79524070683956));
#13016=CARTESIAN_POINT('Ctrl Pts',(7.0418120707574,-0.438413372603167,8.80049373021013));
#13017=CARTESIAN_POINT('Ctrl Pts',(7.07805808635704,-0.235843900652832,
8.81253528393552));
#13018=CARTESIAN_POINT('Ctrl Pts',(7.08849340269679,-0.118748807800604,
8.81925117900009));
#13019=CARTESIAN_POINT('Ctrl Pts',(7.088576988111,-0.000943539479336892,
8.82622343083489));
#13020=CARTESIAN_POINT('Ctrl Pts',(7.08857715545312,-0.000471768392112177,
8.82625135561015));
#13021=CARTESIAN_POINT('Ctrl Pts',(7.08857715545311,2.37118846529926E-11,
8.82627928344061));
#13022=CARTESIAN_POINT('Origin',(5.09382715545311,0.,-6.77268258743872));
#13023=CARTESIAN_POINT('',(7.08857712371941,0.00025895104517608,9.78359198969069));
#13024=CARTESIAN_POINT('',(7.08857665886015,0.00140753592649714,9.62731741260996));
#13025=CARTESIAN_POINT('',(7.08857715545311,8.3550772080578E-14,-6.77268258743872));
#13026=CARTESIAN_POINT('Ctrl Pts',(7.08857709519816,0.000490292911708074,
9.78359207680131));
#13027=CARTESIAN_POINT('Ctrl Pts',(7.08858056938264,-0.0136443786806656,
9.78270707410814));
#13028=CARTESIAN_POINT('Ctrl Pts',(7.08843380748817,-0.0277791914842937,
9.78182936076363));
#13029=CARTESIAN_POINT('Ctrl Pts',(7.08471229123831,-0.204862142831645,
9.77091144180494));
#13030=CARTESIAN_POINT('Ctrl Pts',(7.0613293095822,-0.366799471128801,9.76171666375718));
#13031=CARTESIAN_POINT('Ctrl Pts',(6.9937958317104,-0.614803472615814,9.74667589271688));
#13032=CARTESIAN_POINT('Ctrl Pts',(6.96271955935319,-0.703635144582146,
9.74108856917276));
#13033=CARTESIAN_POINT('Ctrl Pts',(6.91636435148483,-0.811121371616562,
9.73387104510844));
#13034=CARTESIAN_POINT('Ctrl Pts',(6.90686263552512,-0.83214301059918,9.73243718144363));
#13035=CARTESIAN_POINT('Ctrl Pts',(6.89245087133043,-0.862608488093872,
9.73032414307598));
#13036=CARTESIAN_POINT('Ctrl Pts',(6.8878262041889,-0.872185806567827,9.72965474317748));
#13037=CARTESIAN_POINT('Ctrl Pts',(6.87954180212753,-0.888997460646529,
9.72847041339689));
#13038=CARTESIAN_POINT('Ctrl Pts',(6.87591410985923,-0.89624738112057,9.72795660335941));
#13039=CARTESIAN_POINT('Ctrl Pts',(6.86825676563868,-0.911320226460795,
9.72688184340351));
#13040=CARTESIAN_POINT('Ctrl Pts',(6.86421934744489,-0.919138987923251,
9.72632063030293));
#13041=CARTESIAN_POINT('Ctrl Pts',(6.85356339133805,-0.939444335542812,
9.72485334422801));
#13042=CARTESIAN_POINT('Ctrl Pts',(6.84686374989247,-0.951887577942564,
9.72394443242433));
#13043=CARTESIAN_POINT('Ctrl Pts',(6.81864035172033,-1.00299820907502,9.72016985308271));
#13044=CARTESIAN_POINT('Ctrl Pts',(6.79596639209372,-1.04101271731831,9.71726362896545));
#13045=CARTESIAN_POINT('Ctrl Pts',(6.67987439671137,-1.22170362279321,9.70295184442103));
#13046=CARTESIAN_POINT('Ctrl Pts',(6.56969235241088,-1.35274164048764,9.69093381550683));
#13047=CARTESIAN_POINT('Ctrl Pts',(6.40719131537045,-1.50220967333437,9.67565830083682));
#13048=CARTESIAN_POINT('Ctrl Pts',(6.36887988860476,-1.53486172735929,9.67220860034838));
#13049=CARTESIAN_POINT('Ctrl Pts',(6.3147282647795,-1.5775854892631,9.66757575729102));
#13050=CARTESIAN_POINT('Ctrl Pts',(6.29992235910093,-1.58893357584229,9.66633275627732));
#13051=CARTESIAN_POINT('Ctrl Pts',(6.27741574355493,-1.60568802923844,9.66448112299737));
#13052=CARTESIAN_POINT('Ctrl Pts',(6.26983281286004,-1.61125004104356,9.6638636019593));
#13053=CARTESIAN_POINT('Ctrl Pts',(6.25745694076085,-1.62019371834059,9.6628663645966));
#13054=CARTESIAN_POINT('Ctrl Pts',(6.25268801725202,-1.6236081630847,9.66248461512802));
#13055=CARTESIAN_POINT('Ctrl Pts',(6.24351892422364,-1.6301120524599,9.66175556997557));
#13056=CARTESIAN_POINT('Ctrl Pts',(6.239121195777,-1.63320483393593,9.66140805820121));
#13057=CARTESIAN_POINT('Ctrl Pts',(6.23469233951648,-1.63629282061832,9.66106029046108));
#13058=CARTESIAN_POINT('Ctrl Pts',(6.2346737238234,-1.63630579979805,9.66105882873723));
#13059=CARTESIAN_POINT('Ctrl Pts',(6.23463604278237,-1.63633207070898,9.66105587006107));
#13060=CARTESIAN_POINT('Ctrl Pts',(6.23461697748994,-1.63634536237841,9.66105437311503));
#13061=CARTESIAN_POINT('Ctrl Pts',(6.2345783808954,-1.63637226960089,9.66105134271614));
#13062=CARTESIAN_POINT('Ctrl Pts',(6.23455884948748,-1.63638588520322,9.66104980925702));
#13063=CARTESIAN_POINT('Ctrl Pts',(6.23451930333827,-1.63641345229388,9.66104670447797));
#13064=CARTESIAN_POINT('Ctrl Pts',(6.23449928864725,-1.63642740372116,9.66104513316414));
#13065=CARTESIAN_POINT('Ctrl Pts',(6.23445875778972,-1.63645565502901,9.66104195125792));
#13066=CARTESIAN_POINT('Ctrl Pts',(6.23443824156244,-1.63646995492429,9.66104034066303));
#13067=CARTESIAN_POINT('Ctrl Pts',(6.23439668851203,-1.63649891641127,9.66103707870061));
#13068=CARTESIAN_POINT('Ctrl Pts',(6.23437565169313,-1.6365135779706,9.66103542733583));
#13069=CARTESIAN_POINT('Ctrl Pts',(6.23433303731909,-1.63654327673325,9.66103208226002));
#13070=CARTESIAN_POINT('Ctrl Pts',(6.23431145975342,-1.63655831391257,9.66103038855074));
#13071=CARTESIAN_POINT('Ctrl Pts',(6.23426774271571,-1.63658877857337,9.66102695713206));
#13072=CARTESIAN_POINT('Ctrl Pts',(6.23424560317639,-1.63660420606834,9.66102521942013));
#13073=CARTESIAN_POINT('Ctrl Pts',(6.23420073976778,-1.63663546688454,9.66102169824452));
#13074=CARTESIAN_POINT('Ctrl Pts',(6.23417801593563,-1.63665130014424,9.6610199147867));
#13075=CARTESIAN_POINT('Ctrl Pts',(6.23413196034228,-1.63668338882488,9.66101630027611));
#13076=CARTESIAN_POINT('Ctrl Pts',(6.23410862854145,-1.63669964423535,9.66101446922338));
#13077=CARTESIAN_POINT('Ctrl Pts',(6.23406133206577,-1.63673259448129,9.66101075757486));
#13078=CARTESIAN_POINT('Ctrl Pts',(6.2340373673861,-1.63674928927944,9.66100887698207));
#13079=CARTESIAN_POINT('Ctrl Pts',(6.23398877878535,-1.63678313654587,9.66100506419453));
#13080=CARTESIAN_POINT('Ctrl Pts',(6.23396415482753,-1.6368002889962,9.66100313200049));
#13081=CARTESIAN_POINT('Ctrl Pts',(6.23391421977074,-1.6368350708691,9.66099921383216));
#13082=CARTESIAN_POINT('Ctrl Pts',(6.23388890863097,-1.63685270027345,9.66099722785852));
#13083=CARTESIAN_POINT('Ctrl Pts',(6.23383756964423,-1.63688845650577,9.66099319982288));
#13084=CARTESIAN_POINT('Ctrl Pts',(6.23381154175922,-1.63690658331021,9.66099115776204));
#13085=CARTESIAN_POINT('Ctrl Pts',(6.23375873790175,-1.63694335604527,9.66098701510257));
#13086=CARTESIAN_POINT('Ctrl Pts',(6.2337319619427,-1.63696200191286,9.66098491450945));
#13087=CARTESIAN_POINT('Ctrl Pts',(6.233677628672,-1.63699983577588,9.66098065218925));
#13088=CARTESIAN_POINT('Ctrl Pts',(6.23365007134942,-1.63701902372123,9.6609784904661));
#13089=CARTESIAN_POINT('Ctrl Pts',(6.23359414003372,-1.63705796615616,9.66097410312986));
#13090=CARTESIAN_POINT('Ctrl Pts',(6.23356576601462,-1.63707772060176,9.66097187751987));
#13091=CARTESIAN_POINT('Ctrl Pts',(6.23350816374731,-1.63711782199749,9.66096735947955));
#13092=CARTESIAN_POINT('Ctrl Pts',(6.23347893545422,-1.63713816891202,9.66096506705123));
#13093=CARTESIAN_POINT('Ctrl Pts',(6.23341958463795,-1.63717948288866,9.66096041225373));
#13094=CARTESIAN_POINT('Ctrl Pts',(6.23338946207873,-1.63720044990376,9.66095804988769));
#13095=CARTESIAN_POINT('Ctrl Pts',(6.23332828009777,-1.63724303353703,9.66095325188946));
#13096=CARTESIAN_POINT('Ctrl Pts',(6.23329722063836,-1.63726465010355,9.66095081626076));
#13097=CARTESIAN_POINT('Ctrl Pts',(6.22967705170315,-1.63978403952007,9.66066694157444));
#13098=CARTESIAN_POINT('Ctrl Pts',(6.22607979889914,-1.64226996411107,9.66038632171062));
#13099=CARTESIAN_POINT('Ctrl Pts',(6.21772880464628,-1.6480005368209,9.65973820104804));
#13100=CARTESIAN_POINT('Ctrl Pts',(6.21296917595704,-1.65123645379734,9.65937128751451));
#13101=CARTESIAN_POINT('Ctrl Pts',(6.20051530823203,-1.65962484966764,9.658417502493));
#13102=CARTESIAN_POINT('Ctrl Pts',(6.19279897735725,-1.66474450037611,9.65783274392952));
#13103=CARTESIAN_POINT('Ctrl Pts',(6.13936651480117,-1.69966257897415,9.65382400915616));
#13104=CARTESIAN_POINT('Ctrl Pts',(6.09247560886973,-1.72763070594891,9.65050885529362));
#13105=CARTESIAN_POINT('Ctrl Pts',(5.9004466135813,-1.83173130853402,9.63748319666908));
#13106=CARTESIAN_POINT('Ctrl Pts',(5.74732598455105,-1.89177683628475,9.62825747267546));
#13107=CARTESIAN_POINT('Ctrl Pts',(5.52312546357385,-1.9491781367545,9.6144809713942));
#13108=CARTESIAN_POINT('Ctrl Pts',(5.45686969536153,-1.96259805394567,9.61038651847628));
#13109=CARTESIAN_POINT('Ctrl Pts',(5.37463635595553,-1.97494738745605,9.60521385785075));
#13110=CARTESIAN_POINT('Ctrl Pts',(5.35918089712315,-1.9770832962727,9.60423788239153));
#13111=CARTESIAN_POINT('Ctrl Pts',(5.33465200774986,-1.98018033692472,9.60268227035092));
#13112=CARTESIAN_POINT('Ctrl Pts',(5.32559409753436,-1.98126092585779,9.60210638587147));
#13113=CARTESIAN_POINT('Ctrl Pts',(5.30854148282648,-1.9831767266888,9.60101937934311));
#13114=CARTESIAN_POINT('Ctrl Pts',(5.30054849794739,-1.98402582017711,9.60050870355426));
#13115=CARTESIAN_POINT('Ctrl Pts',(5.28255229761046,-1.98582762425466,9.59935619130425));
#13116=CARTESIAN_POINT('Ctrl Pts',(5.27254663413481,-1.98675309849769,9.598713516167));
#13117=CARTESIAN_POINT('Ctrl Pts',(5.24693463544017,-1.98892704059709,9.59706340432625));
#13118=CARTESIAN_POINT('Ctrl Pts',(5.23132004967282,-1.99006742453171,9.59605262991334));
#13119=CARTESIAN_POINT('Ctrl Pts',(5.12697557375343,-1.99645415556563,9.58926492181038));
#13120=CARTESIAN_POINT('Ctrl Pts',(5.03800585766431,-1.99594792476099,9.58331037962471));
#13121=CARTESIAN_POINT('Ctrl Pts',(4.81878094809907,-1.98003087160968,9.56825426549758));
#13122=CARTESIAN_POINT('Ctrl Pts',(4.68944631896635,-1.9577143797468,9.55901893538542));
#13123=CARTESIAN_POINT('Ctrl Pts',(4.50230976806325,-1.90607695918899,9.5456480602962));
#13124=CARTESIAN_POINT('Ctrl Pts',(4.44221021137005,-1.88637728108261,9.5413581719478));
#13125=CARTESIAN_POINT('Ctrl Pts',(4.37370461417087,-1.86025619220699,9.53654793882348));
#13126=CARTESIAN_POINT('Ctrl Pts',(4.36429448228101,-1.85658602389859,9.5358889991515));
#13127=CARTESIAN_POINT('Ctrl Pts',(4.3499122580467,-1.85085038984857,9.53488511188149));
#13128=CARTESIAN_POINT('Ctrl Pts',(4.34492013701131,-1.8488360715766,9.53453725765405));
#13129=CARTESIAN_POINT('Ctrl Pts',(4.33577275985302,-1.84510198044021,9.53390104379138));
#13130=CARTESIAN_POINT('Ctrl Pts',(4.33161517102542,-1.84338836833191,9.53361233537026));
#13131=CARTESIAN_POINT('Ctrl Pts',(4.32226362220931,-1.83949694067467,9.53296396369223));
#13132=CARTESIAN_POINT('Ctrl Pts',(4.31707307659657,-1.83731118306846,9.53260478270446));
#13133=CARTESIAN_POINT('Ctrl Pts',(4.30181944793839,-1.83081163019887,9.5315510989295));
#13134=CARTESIAN_POINT('Ctrl Pts',(4.29178235185806,-1.82643685349128,9.53086014382531));
#13135=CARTESIAN_POINT('Ctrl Pts',(4.20062818028855,-1.78580997186265,9.52460237576486));
#13136=CARTESIAN_POINT('Ctrl Pts',(4.12197095640795,-1.74425379498136,9.51932590898579));
#13137=CARTESIAN_POINT('Ctrl Pts',(3.94705508826657,-1.63632261763769,9.50730098817407));
#13138=CARTESIAN_POINT('Ctrl Pts',(3.85333917991286,-1.56646973547093,9.50062221577276));
#13139=CARTESIAN_POINT('Ctrl Pts',(3.72780610447813,-1.45453399966291,9.49066909945868));
#13140=CARTESIAN_POINT('Ctrl Pts',(3.69069277409877,-1.41876566282053,9.4875822401573));
#13141=CARTESIAN_POINT('Ctrl Pts',(3.63145465382288,-1.35707428007224,9.48236408210045));
#13142=CARTESIAN_POINT('Ctrl Pts',(3.60853402830026,-1.3319489670316,9.48026578004398));
#13143=CARTESIAN_POINT('Ctrl Pts',(3.578160135571,-1.29689411135084,9.47736679987743));
#13144=CARTESIAN_POINT('Ctrl Pts',(3.57013995786508,-1.28746190784513,9.47658950366655));
#13145=CARTESIAN_POINT('Ctrl Pts',(3.55681125577626,-1.27148757459588,9.47527729677973));
#13146=CARTESIAN_POINT('Ctrl Pts',(3.55145536234603,-1.26498528707381,9.47474432206891));
#13147=CARTESIAN_POINT('Ctrl Pts',(3.54096226265785,-1.25208049566206,9.47368870969787));
#13148=CARTESIAN_POINT('Ctrl Pts',(3.53582306915413,-1.24567981707606,9.47316616648768));
#13149=CARTESIAN_POINT('Ctrl Pts',(3.5245855286729,-1.23150554029621,9.47201116258807));
#13150=CARTESIAN_POINT('Ctrl Pts',(3.51850516557976,-1.22371802365883,9.47137800637246));
#13151=CARTESIAN_POINT('Ctrl Pts',(3.49726382693966,-1.1960921828152,9.46913665044792));
#13152=CARTESIAN_POINT('Ctrl Pts',(3.48241823441085,-1.17601537722967,9.46751625563855));
#13153=CARTESIAN_POINT('Ctrl Pts',(3.38512038145608,-1.0391298215808,9.45651984453848));
#13154=CARTESIAN_POINT('Ctrl Pts',(3.31507053328199,-0.914046248028136,
9.44667503502914));
#13155=CARTESIAN_POINT('Ctrl Pts',(3.22361127193429,-0.699611164795465,
9.43042647786043));
#13156=CARTESIAN_POINT('Ctrl Pts',(3.19389125817874,-0.614335779374709,
9.42412306870551));
#13157=CARTESIAN_POINT('Ctrl Pts',(3.16299192542781,-0.501611846912927,
9.41618806453014));
#13158=CARTESIAN_POINT('Ctrl Pts',(3.15645637525136,-0.475745449077102,
9.41439398017825));
#13159=CARTESIAN_POINT('Ctrl Pts',(3.14643835506666,-0.432457659654682,
9.4114441045883));
#13160=CARTESIAN_POINT('Ctrl Pts',(3.14266630746869,-0.415107413588062,
9.41027567582744));
#13161=CARTESIAN_POINT('Ctrl Pts',(3.13778028132236,-0.39109303702865,9.40867973581492));
#13162=CARTESIAN_POINT('Ctrl Pts',(3.1364678676022,-0.384470751620982,9.40824185674323));
#13163=CARTESIAN_POINT('Ctrl Pts',(3.13430729209359,-0.373270865109169,
9.40750519522455));
#13164=CARTESIAN_POINT('Ctrl Pts',(3.13344149647407,-0.368696763301027,
9.40720543445994));
#13165=CARTESIAN_POINT('Ctrl Pts',(3.13181689183311,-0.35994625292207,9.40663412232349));
#13166=CARTESIAN_POINT('Ctrl Pts',(3.13105539197332,-0.355770410303584,
9.40636241480066));
#13167=CARTESIAN_POINT('Ctrl Pts',(3.12927032448868,-0.345801428119675,
9.40571591472891));
#13168=CARTESIAN_POINT('Ctrl Pts',(3.12825903622795,-0.34000608898839,9.40534180751977));
#13169=CARTESIAN_POINT('Ctrl Pts',(3.12474215280575,-0.319311862415041,
9.40401181569426));
#13170=CARTESIAN_POINT('Ctrl Pts',(3.12238012467823,-0.304388649727275,
9.40306358849415));
#13171=CARTESIAN_POINT('Ctrl Pts',(3.10010148894006,-0.15247438414952,9.39350797008247));
#13172=CARTESIAN_POINT('Ctrl Pts',(3.09432419758453,-0.0137696955232201,
9.38556616124658));
#13173=CARTESIAN_POINT('Ctrl Pts',(3.11128240416563,0.25755680127145,9.36977508909929));
#13174=CARTESIAN_POINT('Ctrl Pts',(3.13293257237779,0.389493497569308,9.36196463275907));
#13175=CARTESIAN_POINT('Ctrl Pts',(3.1725849889209,0.536867604732247,9.35251446783645));
#13176=CARTESIAN_POINT('Ctrl Pts',(3.17785640447052,0.555386647847233,9.35131406042808));
#13177=CARTESIAN_POINT('Ctrl Pts',(3.18624168023227,0.583303649203234,9.34948360208502));
#13178=CARTESIAN_POINT('Ctrl Pts',(3.18915887780729,0.592759849276397,9.34885992394804));
#13179=CARTESIAN_POINT('Ctrl Pts',(3.19456932430477,0.609845615308215,9.34772623526088));
#13180=CARTESIAN_POINT('Ctrl Pts',(3.19703850463564,0.617482627085696,9.34721701983474));
#13181=CARTESIAN_POINT('Ctrl Pts',(3.2024461017685,0.63386943731624,9.34611895725713));
#13182=CARTESIAN_POINT('Ctrl Pts',(3.20539928343338,0.642614130931088,9.34552963529677));
#13183=CARTESIAN_POINT('Ctrl Pts',(3.2135336148364,0.666160409487546,9.34393358603061));
#13184=CARTESIAN_POINT('Ctrl Pts',(3.21882871333236,0.680921661336426,9.34292312734048));
#13185=CARTESIAN_POINT('Ctrl Pts',(3.24596467076561,0.753851691292376,9.33788043124632));
#13186=CARTESIAN_POINT('Ctrl Pts',(3.27033891862018,0.811034773642312,9.33376487718167));
#13187=CARTESIAN_POINT('Ctrl Pts',(3.37172755740359,1.02112369187189,9.31802145785408));
#13188=CARTESIAN_POINT('Ctrl Pts',(3.46564442619002,1.16504468483995,9.30587383360492));
#13189=CARTESIAN_POINT('Ctrl Pts',(3.61130597810591,1.33566129315734,9.29050491391615));
#13190=CARTESIAN_POINT('Ctrl Pts',(3.64747237274151,1.3747432732696,9.28691300176108));
#13191=CARTESIAN_POINT('Ctrl Pts',(3.69203359655889,1.41918870126688,9.28278686651145));
#13192=CARTESIAN_POINT('Ctrl Pts',(3.69895515817053,1.42599224117467,9.28215406137601));
#13193=CARTESIAN_POINT('Ctrl Pts',(3.70973224106526,1.43643200632066,9.28118158470513));
#13194=CARTESIAN_POINT('Ctrl Pts',(3.71355294595723,1.44010372855299,9.28083927543976));
#13195=CARTESIAN_POINT('Ctrl Pts',(3.72064754867731,1.44686751570607,9.28020824778634));
#13196=CARTESIAN_POINT('Ctrl Pts',(3.72391726872113,1.44996370415353,9.27991922124559));
#13197=CARTESIAN_POINT('Ctrl Pts',(3.73137697020129,1.45697974397677,9.2792638670414));
#13198=CARTESIAN_POINT('Ctrl Pts',(3.73557339323591,1.4608926042123,9.27889806950475));
#13199=CARTESIAN_POINT('Ctrl Pts',(3.74654294434242,1.47103278996635,9.27794912108883));
#13200=CARTESIAN_POINT('Ctrl Pts',(3.75334246628194,1.47723153918274,9.27736804820794));
#13201=CARTESIAN_POINT('Ctrl Pts',(3.79974471839693,1.51894969481013,9.2734487175258));
#13202=CARTESIAN_POINT('Ctrl Pts',(3.84071547388534,1.55292296076116,9.27021382853565));
#13203=CARTESIAN_POINT('Ctrl Pts',(4.01422392448764,1.6854527125434,9.25718033031886));
#13204=CARTESIAN_POINT('Ctrl Pts',(4.15738888706473,1.76900637772122,9.24788829119936));
#13205=CARTESIAN_POINT('Ctrl Pts',(4.37151336828064,1.86061301819059,9.23402615948148));
#13206=CARTESIAN_POINT('Ctrl Pts',(4.43511645045457,1.88406920465866,9.22992064547232));
#13207=CARTESIAN_POINT('Ctrl Pts',(4.51469103213906,1.90889306332427,9.22473555252779));
#13208=CARTESIAN_POINT('Ctrl Pts',(4.5296508464989,1.91336782851897,9.22375881523377));
#13209=CARTESIAN_POINT('Ctrl Pts',(4.55343357211658,1.9201785335369,9.22220226671657));
#13210=CARTESIAN_POINT('Ctrl Pts',(4.56222283199847,1.9226304024417,9.22162621544305));
#13211=CARTESIAN_POINT('Ctrl Pts',(4.57878515899622,1.92712840981505,9.22053906609375));
#13212=CARTESIAN_POINT('Ctrl Pts',(4.58655439600613,1.92918804435095,9.220028415565));
#13213=CARTESIAN_POINT('Ctrl Pts',(4.60406012394034,1.93371577698622,9.21887619012968));
#13214=CARTESIAN_POINT('Ctrl Pts',(4.61380317943314,1.9361573871178,9.21823377831003));
#13215=CARTESIAN_POINT('Ctrl Pts',(4.63876593118917,1.94221305206307,9.21658479353995));
#13216=CARTESIAN_POINT('Ctrl Pts',(4.65401022985351,1.94572179572118,9.21557489062507));
#13217=CARTESIAN_POINT('Ctrl Pts',(4.75576409181738,1.96788535423448,9.208813282744));
#13218=CARTESIAN_POINT('Ctrl Pts',(4.84337972908982,1.98094211418654,9.20288557826055));
#13219=CARTESIAN_POINT('Ctrl Pts',(5.07638100322952,1.99995881899078,9.18687517736236));
#13220=CARTESIAN_POINT('Ctrl Pts',(5.22204591425514,1.99591982084095,9.17659012793101));
#13221=CARTESIAN_POINT('Ctrl Pts',(5.41571784836937,1.96924738150639,9.16322156967735));
#13222=CARTESIAN_POINT('Ctrl Pts',(5.46518936716049,1.96052031732577,9.15983880124491));
#13223=CARTESIAN_POINT('Ctrl Pts',(5.52363081081484,1.94791884449774,9.15592044176644));
#13224=CARTESIAN_POINT('Ctrl Pts',(5.53296423654172,1.94583597450386,9.15529705678845));
#13225=CARTESIAN_POINT('Ctrl Pts',(5.54741591761246,1.94250162204944,9.154335925822));
#13226=CARTESIAN_POINT('Ctrl Pts',(5.55254465176657,1.94129688016715,9.15399563628537));
#13227=CARTESIAN_POINT('Ctrl Pts',(5.56205145050944,1.93902395013897,9.15336643493351));
#13228=CARTESIAN_POINT('Ctrl Pts',(5.56643064118469,1.93796125234192,9.15307722994925));
#13229=CARTESIAN_POINT('Ctrl Pts',(5.57641814168836,1.93550171913232,9.15241905093835));
#13230=CARTESIAN_POINT('Ctrl Pts',(5.58202400396105,1.93409534508421,9.15205062595321));
#13231=CARTESIAN_POINT('Ctrl Pts',(5.59667348040336,1.93035239781506,9.15109027859986));
#13232=CARTESIAN_POINT('Ctrl Pts',(5.60570705591467,1.92797660299644,9.1505005169776));
#13233=CARTESIAN_POINT('Ctrl Pts',(5.66928952027276,1.91077626534526,9.14636454296859));
#13234=CARTESIAN_POINT('Ctrl Pts',(5.72320870401148,1.89370087524915,9.14293517080237));
#13235=CARTESIAN_POINT('Ctrl Pts',(5.92859991479799,1.81891198074968,9.12991935822585));
#13236=CARTESIAN_POINT('Ctrl Pts',(6.0735445964106,1.74512042158038,9.12078764113241));
#13237=CARTESIAN_POINT('Ctrl Pts',(6.26378708595887,1.61701864263524,9.10713270216937));
#13238=CARTESIAN_POINT('Ctrl Pts',(6.31766017312476,1.57663783125968,9.10305428042643));
#13239=CARTESIAN_POINT('Ctrl Pts',(6.38136796813201,1.52364992181965,9.09789963969131));
#13240=CARTESIAN_POINT('Ctrl Pts',(6.39323200251213,1.5135446641578,9.09692477334345));
#13241=CARTESIAN_POINT('Ctrl Pts',(6.41184791224716,1.4973082478483,9.09537052467234));
#13242=CARTESIAN_POINT('Ctrl Pts',(6.41867839791675,1.49126787845384,9.09479488303838));
#13243=CARTESIAN_POINT('Ctrl Pts',(6.43145216248658,1.47981469127294,9.09370808407573));
#13244=CARTESIAN_POINT('Ctrl Pts',(6.43740461995159,1.47441234861633,9.09319737113171));
#13245=CARTESIAN_POINT('Ctrl Pts',(6.45072837455823,1.46217226511459,9.09204443948996));
#13246=CARTESIAN_POINT('Ctrl Pts',(6.45808091142421,1.45531451394619,9.09140137953981));
#13247=CARTESIAN_POINT('Ctrl Pts',(6.47676322007462,1.43762342874743,9.08974962024798));
#13248=CARTESIAN_POINT('Ctrl Pts',(6.48801753812336,1.42671175624055,9.08873757186156));
#13249=CARTESIAN_POINT('Ctrl Pts',(6.5626221999405,1.35265275062906,9.08191189022883));
#13250=CARTESIAN_POINT('Ctrl Pts',(6.62178324286563,1.28544723489754,9.07591829454578));
#13251=CARTESIAN_POINT('Ctrl Pts',(6.75564465433856,1.11103694458457,9.06085433178684));
#13252=CARTESIAN_POINT('Ctrl Pts',(6.82471376230149,1.00003446359356,9.05165506144627));
#13253=CARTESIAN_POINT('Ctrl Pts',(6.91039312417284,0.826498006955609,9.03832574008705));
#13254=CARTESIAN_POINT('Ctrl Pts',(6.93563543445955,0.768605767662508,9.03404214709338));
#13255=CARTESIAN_POINT('Ctrl Pts',(6.96168395794934,0.700171749112511,9.02923802531838));
#13256=CARTESIAN_POINT('Ctrl Pts',(6.9652042514705,0.690707816397884,9.02857928952517));
#13257=CARTESIAN_POINT('Ctrl Pts',(6.97049074950568,0.676158478411955,9.02757564690223));
#13258=CARTESIAN_POINT('Ctrl Pts',(6.97230842386432,0.671092139014209,9.02722783558428));
#13259=CARTESIAN_POINT('Ctrl Pts',(6.97560706783441,0.66177953018706,9.02659166274013));
#13260=CARTESIAN_POINT('Ctrl Pts',(6.97709418342905,0.657535616790079,9.02630295273997));
#13261=CARTESIAN_POINT('Ctrl Pts',(6.98041169206445,0.647964563429164,9.02565453099698));
#13262=CARTESIAN_POINT('Ctrl Pts',(6.98223387850055,0.642634685849197,9.02529530187292));
#13263=CARTESIAN_POINT('Ctrl Pts',(6.98753257020638,0.626918906040165,9.02424134427596));
#13264=CARTESIAN_POINT('Ctrl Pts',(6.99094621120514,0.616511811453599,9.02355016624073));
#13265=CARTESIAN_POINT('Ctrl Pts',(7.02195676509225,0.519273465365948,9.01715038345162));
#13266=CARTESIAN_POINT('Ctrl Pts',(7.04366360600454,0.430663346349435,9.01174733098971));
#13267=CARTESIAN_POINT('Ctrl Pts',(7.07867991309622,0.228763564477506,8.99976859373272));
#13268=CARTESIAN_POINT('Ctrl Pts',(7.08849541674042,0.115202496718061,8.99324927811289));
#13269=CARTESIAN_POINT('Ctrl Pts',(7.0885769860218,0.000949408244314996,
8.98649007198198));
#13270=CARTESIAN_POINT('Ctrl Pts',(7.08857715545312,0.000474702745457553,
8.98646198520671));
#13271=CARTESIAN_POINT('Ctrl Pts',(7.08857715545311,-2.42987105381791E-11,
8.98643389536847));
#13272=CARTESIAN_POINT('Ctrl Pts',(7.08857715545311,2.37118846529926E-11,
8.82627928344061));
#13273=CARTESIAN_POINT('Ctrl Pts',(7.08857715545221,0.0760979497660257,
8.83078414338272));
#13274=CARTESIAN_POINT('Ctrl Pts',(7.08422265935748,0.152126168627862,8.835372281333));
#13275=CARTESIAN_POINT('Ctrl Pts',(7.07380624533671,0.242776038297638,8.84103906841134));
#13276=CARTESIAN_POINT('Ctrl Pts',(7.07190396794442,0.257816805620438,8.84198571175015));
#13277=CARTESIAN_POINT('Ctrl Pts',(7.0684768006953,0.282638092816422,8.84355918120427));
#13278=CARTESIAN_POINT('Ctrl Pts',(7.06705020351653,0.292431718342481,8.8441829234237));
#13279=CARTESIAN_POINT('Ctrl Pts',(7.06433477441333,0.310147881550535,8.84531668026858));
#13280=CARTESIAN_POINT('Ctrl Pts',(7.06307088492161,0.31807407265161,8.84582589931603));
#13281=CARTESIAN_POINT('Ctrl Pts',(7.06025093466268,0.335097388987296,8.84692391548401));
#13282=CARTESIAN_POINT('Ctrl Pts',(7.05867951050679,0.344191745515105,8.84751318705433));
#13283=CARTESIAN_POINT('Ctrl Pts',(7.05419493632479,0.369113414579321,8.84913551434706));
#13284=CARTESIAN_POINT('Ctrl Pts',(7.05115332234949,0.384916614859681,8.85017260581042));
#13285=CARTESIAN_POINT('Ctrl Pts',(7.03271965249735,0.47481637841628,8.85612140679021));
#13286=CARTESIAN_POINT('Ctrl Pts',(7.01331377466768,0.548017677217242,8.86115962069973));
#13287=CARTESIAN_POINT('Ctrl Pts',(6.95485744178155,0.726797709814179,8.87394924089058));
#13288=CARTESIAN_POINT('Ctrl Pts',(6.91094503843883,0.830510371622907,8.88181566906143));
#13289=CARTESIAN_POINT('Ctrl Pts',(6.81398859389791,1.01449628934127,8.89628916999919));
#13290=CARTESIAN_POINT('Ctrl Pts',(6.76341882492772,1.09573082704069,8.90288524759426));
#13291=CARTESIAN_POINT('Ctrl Pts',(6.70077471736184,1.18189128282182,8.90988690350465));
#13292=CARTESIAN_POINT('Ctrl Pts',(6.69426228995225,1.19069511812867,8.91060232555328));
#13293=CARTESIAN_POINT('Ctrl Pts',(6.68429084625799,1.20394540279637,8.91167851831354));
#13294=CARTESIAN_POINT('Ctrl Pts',(6.68088507665168,1.20843139702795,8.9120427739568));
#13295=CARTESIAN_POINT('Ctrl Pts',(6.67472595970842,1.21647308046997,8.91269547785338));
#13296=CARTESIAN_POINT('Ctrl Pts',(6.67197956142243,1.22003392146302,8.91298439192521));
#13297=CARTESIAN_POINT('Ctrl Pts',(6.66591923884948,1.22783672294277,8.91361725701998));
#13298=CARTESIAN_POINT('Ctrl Pts',(6.66260018139192,1.23207456414338,8.91396084101251));
#13299=CARTESIAN_POINT('Ctrl Pts',(6.6530050411444,1.24422420269283,8.91494565132783));
#13300=CARTESIAN_POINT('Ctrl Pts',(6.64668587034087,1.25210197966945,8.91558392275841));
#13301=CARTESIAN_POINT('Ctrl Pts',(6.60041323684749,1.30889847037254,8.92018647651089));
#13302=CARTESIAN_POINT('Ctrl Pts',(6.55821184370865,1.35594838761058,8.92400395321448));
#13303=CARTESIAN_POINT('Ctrl Pts',(6.42201128856213,1.49400554635726,8.93550538715055));
#13304=CARTESIAN_POINT('Ctrl Pts',(6.32124600335177,1.57783756365826,8.94294624494332));
#13305=CARTESIAN_POINT('Ctrl Pts',(6.13925826234273,1.7011868816636,8.95587898018585));
#13306=CARTESIAN_POINT('Ctrl Pts',(6.06226250357025,1.74616525125904,8.96121628034075));
#13307=CARTESIAN_POINT('Ctrl Pts',(5.96850265769208,1.79282337478631,8.96771574529454));
#13308=CARTESIAN_POINT('Ctrl Pts',(5.95439875500756,1.799635904198,8.96869323865727));
#13309=CARTESIAN_POINT('Ctrl Pts',(5.93111551755111,1.81054598757118,8.9703073342681));
#13310=CARTESIAN_POINT('Ctrl Pts',(5.9219826771311,1.81474157950974,8.97094056426278));
#13311=CARTESIAN_POINT('Ctrl Pts',(5.90548923246542,1.82216817207927,8.97208450831558));
#13312=CARTESIAN_POINT('Ctrl Pts',(5.89814001994176,1.82542405690789,8.97259435960373));
#13313=CARTESIAN_POINT('Ctrl Pts',(5.88241018807183,1.83227933229988,8.97368598538797));
#13314=CARTESIAN_POINT('Ctrl Pts',(5.87402418296078,1.83586582969306,8.97426818345401));
#13315=CARTESIAN_POINT('Ctrl Pts',(5.85123279958213,1.84542880722114,8.97585123020299));
#13316=CARTESIAN_POINT('Ctrl Pts',(5.83678168750217,1.85129396173417,8.97685579495235));
#13317=CARTESIAN_POINT('Ctrl Pts',(5.75945496379858,1.8816267248029,8.98223666026397));
#13318=CARTESIAN_POINT('Ctrl Pts',(5.69544365968772,1.90305946659127,8.98671247759826));
#13319=CARTESIAN_POINT('Ctrl Pts',(5.473269407412,1.96511912721978,9.00232246334067));
#13320=CARTESIAN_POINT('Ctrl Pts',(5.31127170631543,1.98956711685327,9.0138902050785));
#13321=CARTESIAN_POINT('Ctrl Pts',(5.09289195806131,1.99551528072559,9.02888123939717));
#13322=CARTESIAN_POINT('Ctrl Pts',(5.03760015232606,1.99472349654567,9.03261826235321));
#13323=CARTESIAN_POINT('Ctrl Pts',(4.97313342366823,1.9911169897593,9.03685610531516));
#13324=CARTESIAN_POINT('Ctrl Pts',(4.96386267486578,1.99053336709388,9.03746263177369));
#13325=CARTESIAN_POINT('Ctrl Pts',(4.94884619986041,1.98948267360683,9.0384399950554));
#13326=CARTESIAN_POINT('Ctrl Pts',(4.94309795245298,1.98905542794523,9.0388129207009));
#13327=CARTESIAN_POINT('Ctrl Pts',(4.9328603819417,1.98824987258025,9.03947485346613));
#13328=CARTESIAN_POINT('Ctrl Pts',(4.92837041459726,1.9878812656327,9.03976438704435));
#13329=CARTESIAN_POINT('Ctrl Pts',(4.91862140371193,1.98704765391972,9.04039135086999));
#13330=CARTESIAN_POINT('Ctrl Pts',(4.91336294831854,1.98657698211864,9.04072846365312));
#13331=CARTESIAN_POINT('Ctrl Pts',(4.89853375228362,1.9851902893926,9.04167630579501));
#13332=CARTESIAN_POINT('Ctrl Pts',(4.88896752370563,1.98422592928882,9.04228441539479));
#13333=CARTESIAN_POINT('Ctrl Pts',(4.82843013702353,1.97768074990426,9.04611364248889));
#13334=CARTESIAN_POINT('Ctrl Pts',(4.77767841846249,1.97020498653982,9.04923848047464));
#13335=CARTESIAN_POINT('Ctrl Pts',(4.57638209666626,1.93257341706803,9.06148933290478));
#13336=CARTESIAN_POINT('Ctrl Pts',(4.42925148129793,1.88704385505036,9.07015789140508));
#13337=CARTESIAN_POINT('Ctrl Pts',(4.21577461234178,1.79288035495328,9.08394381316185));
#13338=CARTESIAN_POINT('Ctrl Pts',(4.14476461206291,1.75632409323216,9.08874687082529));
#13339=CARTESIAN_POINT('Ctrl Pts',(4.06298031694305,1.70781043019178,9.0946512422459));
#13340=CARTESIAN_POINT('Ctrl Pts',(4.04991136331929,1.69985336678142,9.09560649252288));
#13341=CARTESIAN_POINT('Ctrl Pts',(4.02850546524009,1.686480376724,9.09719130245843));
#13342=CARTESIAN_POINT('Ctrl Pts',(4.02011502125607,1.68115097830449,9.0978176989037));
#13343=CARTESIAN_POINT('Ctrl Pts',(4.00501956260879,1.67140361923066,9.09895428425956));
#13344=CARTESIAN_POINT('Ctrl Pts',(3.9983006873012,1.66700743463307,9.09946365878022));
#13345=CARTESIAN_POINT('Ctrl Pts',(3.98394269266574,1.65748865363546,9.10055978438395));
#13346=CARTESIAN_POINT('Ctrl Pts',(3.9763121190566,1.65235356278161,9.1011469952109));
#13347=CARTESIAN_POINT('Ctrl Pts',(3.95554848108372,1.63817079579533,9.10275785618563));
#13348=CARTESIAN_POINT('Ctrl Pts',(3.94248820141562,1.62901825809904,9.10378544757433));
#13349=CARTESIAN_POINT('Ctrl Pts',(3.8701535440139,1.57702231991211,9.10955899788924));
#13350=CARTESIAN_POINT('Ctrl Pts',(3.81316732380429,1.53110570448652,9.11442274949977));
#13351=CARTESIAN_POINT('Ctrl Pts',(3.61247074237118,1.35033805252826,9.13276218955385));
#13352=CARTESIAN_POINT('Ctrl Pts',(3.48645868926604,1.19757455498695,9.14689395726083));
#13353=CARTESIAN_POINT('Ctrl Pts',(3.37418982158714,1.01109060527131,9.16140627367036));
#13354=CARTESIAN_POINT('Ctrl Pts',(3.36378099166898,0.993175273625215,9.16277416484257));
#13355=CARTESIAN_POINT('Ctrl Pts',(3.35003282845752,0.968640151642241,9.16460882973998));
#13356=CARTESIAN_POINT('Ctrl Pts',(3.346448893022,0.962159867370846,9.16508979893298));
#13357=CARTESIAN_POINT('Ctrl Pts',(3.34083303921776,0.951870697021146,9.16584759161114));
#13358=CARTESIAN_POINT('Ctrl Pts',(3.3387772980346,0.948074993995554,9.1661258864888));
#13359=CARTESIAN_POINT('Ctrl Pts',(3.33455709681111,0.940222084572862,9.16669901085324));
#13360=CARTESIAN_POINT('Ctrl Pts',(3.33239433332008,0.93616404601662,9.16699372195623));
#13361=CARTESIAN_POINT('Ctrl Pts',(3.32723235133456,0.926397292947214,9.16769961272918));
#13362=CARTESIAN_POINT('Ctrl Pts',(3.32424671266118,0.920681381132768,9.16810994574711));
#13363=CARTESIAN_POINT('Ctrl Pts',(3.3140354567574,0.900899072733677,9.16952083754897));
#13364=CARTESIAN_POINT('Ctrl Pts',(3.30694920314536,0.886760875499597,9.17051313686825));
#13365=CARTESIAN_POINT('Ctrl Pts',(3.26519662890606,0.800924540663502,9.17645029898195));
#13366=CARTESIAN_POINT('Ctrl Pts',(3.23467754965281,0.727279392004382,9.1811808851516));
#13367=CARTESIAN_POINT('Ctrl Pts',(3.1934935346287,0.608200205706659,9.18855867868733));
#13368=CARTESIAN_POINT('Ctrl Pts',(3.17987627503896,0.56388609139749,9.19124720347536));
#13369=CARTESIAN_POINT('Ctrl Pts',(3.13236526242235,0.387619044713416,9.20184428856065));
#13370=CARTESIAN_POINT('Ctrl Pts',(3.11048366598882,0.25283234994045,9.2097667027817));
#13371=CARTESIAN_POINT('Ctrl Pts',(3.10106095662865,0.0922878943931453,
9.2196612316521));
#13372=CARTESIAN_POINT('Ctrl Pts',(3.10007342597037,0.0676768962468813,
9.22118954601111));
#13373=CARTESIAN_POINT('Ctrl Pts',(3.09932401521739,0.03296436106125,9.22336401478594));
#13374=CARTESIAN_POINT('Ctrl Pts',(3.0991827605493,0.0228726348444884,9.22399842265227));
#13375=CARTESIAN_POINT('Ctrl Pts',(3.09906996070037,0.00526734985763139,
9.22510925584522));
#13376=CARTESIAN_POINT('Ctrl Pts',(3.09906427112982,-0.00224584441580045,
9.2255846122532));
#13377=CARTESIAN_POINT('Ctrl Pts',(3.09914133289803,-0.0179974714150017,
9.22658401629271));
#13378=CARTESIAN_POINT('Ctrl Pts',(3.09923267930035,-0.0262357017633881,
9.22710832219145));
#13379=CARTESIAN_POINT('Ctrl Pts',(3.09957266627717,-0.0459057957901291,
9.22836413746277));
#13380=CARTESIAN_POINT('Ctrl Pts',(3.09986857207116,-0.0573364496693194,
9.22909710336108));
#13381=CARTESIAN_POINT('Ctrl Pts',(3.10121707771109,-0.096431662920323,
9.2316152549893));
#13382=CARTESIAN_POINT('Ctrl Pts',(3.10274726524423,-0.124075505898767,
9.23341516284926));
#13383=CARTESIAN_POINT('Ctrl Pts',(3.10782508414471,-0.190661902722997,
9.23779946483038));
#13384=CARTESIAN_POINT('Ctrl Pts',(3.1119433354543,-0.229548196846885,9.24040044888724));
#13385=CARTESIAN_POINT('Ctrl Pts',(3.13280924536336,-0.383279842485552,
9.25084352172333));
#13386=CARTESIAN_POINT('Ctrl Pts',(3.15842089913588,-0.496680837974895,
9.25892172714264));
#13387=CARTESIAN_POINT('Ctrl Pts',(3.22486205567496,-0.70459293903088,9.27413646645248));
#13388=CARTESIAN_POINT('Ctrl Pts',(3.26343090228397,-0.799459477458545,
9.28124378889092));
#13389=CARTESIAN_POINT('Ctrl Pts',(3.31640767013586,-0.905579715879931,
9.28910683041745));
#13390=CARTESIAN_POINT('Ctrl Pts',(3.32388689301532,-0.920112035050285,
9.29018141595129));
#13391=CARTESIAN_POINT('Ctrl Pts',(3.33469378866268,-0.940490592871772,
9.29168348457136));
#13392=CARTESIAN_POINT('Ctrl Pts',(3.33787347857867,-0.94641399252528,9.29211950691601));
#13393=CARTESIAN_POINT('Ctrl Pts',(3.34328088132122,-0.956366298440255,
9.29285097176382));
#13394=CARTESIAN_POINT('Ctrl Pts',(3.34549268662557,-0.960403738683668,
9.29314739700613));
#13395=CARTESIAN_POINT('Ctrl Pts',(3.35004932808787,-0.968653546099105,
9.29375239096686));
#13396=CARTESIAN_POINT('Ctrl Pts',(3.35239548619422,-0.972865122244218,
9.29406087335462));
#13397=CARTESIAN_POINT('Ctrl Pts',(3.35844608601426,-0.983634501491481,
9.29484884699529));
#13398=CARTESIAN_POINT('Ctrl Pts',(3.36217248194113,-0.990179975922129,
9.29532696091645));
#13399=CARTESIAN_POINT('Ctrl Pts',(3.37776430662929,-1.01721003561123,9.29729869049969));
#13400=CARTESIAN_POINT('Ctrl Pts',(3.38995738761668,-1.03750464481498,9.29877268952594));
#13401=CARTESIAN_POINT('Ctrl Pts',(3.42353875935214,-1.09120918983404,9.30266924859209));
#13402=CARTESIAN_POINT('Ctrl Pts',(3.44556777915511,-1.1242073823748,9.30505926463014));
#13403=CARTESIAN_POINT('Ctrl Pts',(3.52259727882864,-1.23245627405984,9.31296181766228));
#13404=CARTESIAN_POINT('Ctrl Pts',(3.58188390471015,-1.30450798586023,9.3183309009443));
#13405=CARTESIAN_POINT('Ctrl Pts',(3.73555534470127,-1.46665510003005,9.33131554380514));
#13406=CARTESIAN_POINT('Ctrl Pts',(3.83414113913017,-1.55214826217755,9.33896163386031));
#13407=CARTESIAN_POINT('Ctrl Pts',(3.95356478482326,-1.63679316161392,9.34803926752736));
#13408=CARTESIAN_POINT('Ctrl Pts',(3.9668981282197,-1.64600154049722,9.3490499587622));
#13409=CARTESIAN_POINT('Ctrl Pts',(3.9888166389429,-1.66074791930276,9.350707700327));
#13410=CARTESIAN_POINT('Ctrl Pts',(3.99733493892073,-1.66638432119765,9.35135105546176));
#13411=CARTESIAN_POINT('Ctrl Pts',(4.01264673484449,-1.67634761549912,9.35250608373521));
#13412=CARTESIAN_POINT('Ctrl Pts',(4.01942390282066,-1.68069928230313,9.35301682243748));
#13413=CARTESIAN_POINT('Ctrl Pts',(4.03384459688311,-1.68983604430843,9.35410265339705));
#13414=CARTESIAN_POINT('Ctrl Pts',(4.04149456995901,-1.694610576574,9.35467811958011));
#13415=CARTESIAN_POINT('Ctrl Pts',(4.06206172425826,-1.70725406082268,9.35622395387176));
#13416=CARTESIAN_POINT('Ctrl Pts',(4.07503626793683,-1.71502811635564,9.35719774565479));
#13417=CARTESIAN_POINT('Ctrl Pts',(4.14059247829747,-1.75330151593455,9.36211216540894));
#13418=CARTESIAN_POINT('Ctrl Pts',(4.19445555233717,-1.78153079575272,9.36613278910501));
#13419=CARTESIAN_POINT('Ctrl Pts',(4.36590098780595,-1.86162619808905,9.37888405024058));
#13420=CARTESIAN_POINT('Ctrl Pts',(4.48725283064651,-1.90462315719648,9.38786672760109));
#13421=CARTESIAN_POINT('Ctrl Pts',(4.70526344586078,-1.95890462597907,9.40350397943443));
#13422=CARTESIAN_POINT('Ctrl Pts',(4.80022096742692,-1.9753705601034,9.41014932078351));
#13423=CARTESIAN_POINT('Ctrl Pts',(4.90690254671284,-1.98600268619209,9.41719590674751));
#13424=CARTESIAN_POINT('Ctrl Pts',(4.91780825444627,-1.98699895277892,9.41791135234793));
#13425=CARTESIAN_POINT('Ctrl Pts',(4.93433489835356,-1.98837157127777,9.41898757340141));
#13426=CARTESIAN_POINT('Ctrl Pts',(4.93994992586598,-1.98881398970185,9.41935183405247));
#13427=CARTESIAN_POINT('Ctrl Pts',(4.95005132119147,-1.98956686098157,9.42000454319236));
#13428=CARTESIAN_POINT('Ctrl Pts',(4.9545369111246,-1.98988592985929,9.42029345753496));
#13429=CARTESIAN_POINT('Ctrl Pts',(4.96439410300606,-1.99055359664685,9.42092631882941));
#13430=CARTESIAN_POINT('Ctrl Pts',(4.96976604529517,-1.99089562226996,9.42126989878135));
#13431=CARTESIAN_POINT('Ctrl Pts',(4.98521986352393,-1.9918167575792,9.42225468584763));
#13432=CARTESIAN_POINT('Ctrl Pts',(4.99530501221645,-1.9923410694518,9.42289293828642));
#13433=CARTESIAN_POINT('Ctrl Pts',(5.06848361258688,-1.99558848725332,9.42749491824918));
#13434=CARTESIAN_POINT('Ctrl Pts',(5.131677675699,-1.99539087944476,9.43131188180093));
#13435=CARTESIAN_POINT('Ctrl Pts',(5.32725024375857,-1.98548215522978,9.44292544165388));
#13436=CARTESIAN_POINT('Ctrl Pts',(5.45874131759604,-1.96557019456372,9.45047012875908));
#13437=CARTESIAN_POINT('Ctrl Pts',(5.67181894277521,-1.91116838431199,9.46341675945952));
#13438=CARTESIAN_POINT('Ctrl Pts',(5.75483485760147,-1.88406612541645,9.46864839780292));
#13439=CARTESIAN_POINT('Ctrl Pts',(5.85031925129852,-1.84580383195983,9.47503251129424));
#13440=CARTESIAN_POINT('Ctrl Pts',(5.86476498519205,-1.83981708823951,9.47600841563369));
#13441=CARTESIAN_POINT('Ctrl Pts',(5.88837011826137,-1.82970759861217,9.47762042018723));
#13442=CARTESIAN_POINT('Ctrl Pts',(5.89757158047095,-1.82568434005061,9.47825316327613));
#13443=CARTESIAN_POINT('Ctrl Pts',(5.91408191052871,-1.81831633672508,9.47939657954902));
#13444=CARTESIAN_POINT('Ctrl Pts',(5.92140173058969,-1.81499655182456,9.47990639340876));
#13445=CARTESIAN_POINT('Ctrl Pts',(5.92884967517527,-1.81156423589755,9.48042812604344));
#13446=CARTESIAN_POINT('Ctrl Pts',(5.92899814071914,-1.81149579480493,9.4804385273545));
#13447=CARTESIAN_POINT('Ctrl Pts',(5.92928339003147,-1.81136425527705,9.48045851390645));
#13448=CARTESIAN_POINT('Ctrl Pts',(5.9294201750788,-1.8113011595933,9.48046809905304));
#13449=CARTESIAN_POINT('Ctrl Pts',(5.92968300903404,-1.81117988444209,9.48048651900443));
#13450=CARTESIAN_POINT('Ctrl Pts',(5.92980905902013,-1.81112170730783,9.48049535372895));
#13451=CARTESIAN_POINT('Ctrl Pts',(5.93005128995293,-1.81100987732168,9.48051233315567));
#13452=CARTESIAN_POINT('Ctrl Pts',(5.93016747181586,-1.81095622644582,9.48052047778998));
#13453=CARTESIAN_POINT('Ctrl Pts',(5.9303907614827,-1.81085308887491,9.48053613238079));
#13454=CARTESIAN_POINT('Ctrl Pts',(5.93049787005777,-1.81080360385768,9.48054364227931));
#13455=CARTESIAN_POINT('Ctrl Pts',(5.93070374196281,-1.81070846722772,9.48055807817218));
#13456=CARTESIAN_POINT('Ctrl Pts',(5.93080250595016,-1.81066281703651,9.48056500411757));
#13457=CARTESIAN_POINT('Ctrl Pts',(5.93099235691375,-1.81057504623099,9.48057831868741));
#13458=CARTESIAN_POINT('Ctrl Pts',(5.93108344444756,-1.81053292682299,9.48058470727029));
#13459=CARTESIAN_POINT('Ctrl Pts',(5.93125855526064,-1.81045193851897,9.48059698985632));
#13460=CARTESIAN_POINT('Ctrl Pts',(5.93134257902751,-1.81041307064042,9.48060288382517));
#13461=CARTESIAN_POINT('Ctrl Pts',(5.93150412438894,-1.81033832901781,9.48061421641117));
#13462=CARTESIAN_POINT('Ctrl Pts',(5.93158164638699,-1.81030245614279,9.48061965499843));
#13463=CARTESIAN_POINT('Ctrl Pts',(5.93173070388572,-1.81023346898623,9.48063011282872));
#13464=CARTESIAN_POINT('Ctrl Pts',(5.9318022397345,-1.81020035544066,9.48063513204671));
#13465=CARTESIAN_POINT('Ctrl Pts',(5.93193979827163,-1.81013667045927,9.48064478420504));
#13466=CARTESIAN_POINT('Ctrl Pts',(5.93200582123244,-1.8101060996599,9.48064941712247));
#13467=CARTESIAN_POINT('Ctrl Pts',(5.93213278846033,-1.81004730122706,9.48065832704396));
#13468=CARTESIAN_POINT('Ctrl Pts',(5.93219373299605,-1.81001907411771,9.48066260403112));
#13469=CARTESIAN_POINT('Ctrl Pts',(5.93231094247213,-1.80996478011355,9.48067082999567));
#13470=CARTESIAN_POINT('Ctrl Pts',(5.93236720762715,-1.80993871367104,9.4806747789577));
#13471=CARTESIAN_POINT('Ctrl Pts',(5.93250999999545,-1.80987255293429,9.48068480126619));
#13472=CARTESIAN_POINT('Ctrl Pts',(5.93259652554851,-1.80983245505883,9.48069087473609));
#13473=CARTESIAN_POINT('Ctrl Pts',(5.93276809181106,-1.80975293247147,9.48070291827513));
#13474=CARTESIAN_POINT('Ctrl Pts',(5.93285313261335,-1.80971350797206,9.48070888833669));
#13475=CARTESIAN_POINT('Ctrl Pts',(5.93302176367064,-1.80963531699865,9.48072072742483));
#13476=CARTESIAN_POINT('Ctrl Pts',(5.93310535401702,-1.80959655072767,9.4807265964443));
#13477=CARTESIAN_POINT('Ctrl Pts',(5.94188974115152,-1.80552192047103,9.48134340392352));
#13478=CARTESIAN_POINT('Ctrl Pts',(5.95056119154166,-1.80142342070975,9.48195649054254));
#13479=CARTESIAN_POINT('Ctrl Pts',(5.97546048355993,-1.78943450129263,9.48372926714405));
#13480=CARTESIAN_POINT('Ctrl Pts',(5.99161091641285,-1.78138638224235,9.48489438020845));
#13481=CARTESIAN_POINT('Ctrl Pts',(6.02793467326662,-1.76266601802192,9.4875502764903));
#13482=CARTESIAN_POINT('Ctrl Pts',(6.04803821000352,-1.75186458917444,9.48904542108051));
#13483=CARTESIAN_POINT('Ctrl Pts',(6.11276662779995,-1.71564194454389,9.4939431761243));
#13484=CARTESIAN_POINT('Ctrl Pts',(6.15659329920891,-1.68884348774038,9.49739175985414));
#13485=CARTESIAN_POINT('Ctrl Pts',(6.29726581779495,-1.59518183063793,9.50889579464913));
#13486=CARTESIAN_POINT('Ctrl Pts',(6.38923092549112,-1.52144496764536,9.5171439812789));
#13487=CARTESIAN_POINT('Ctrl Pts',(6.53779882822161,-1.37903795842688,9.53144564528473));
#13488=CARTESIAN_POINT('Ctrl Pts',(6.59733706958975,-1.31387269477853,9.53751019681739));
#13489=CARTESIAN_POINT('Ctrl Pts',(6.6592029196654,-1.23642469282774,9.54402521966077));
#13490=CARTESIAN_POINT('Ctrl Pts',(6.66596222848696,-1.22781864673421,9.54474013625047));
#13491=CARTESIAN_POINT('Ctrl Pts',(6.67609188756291,-1.21470061488759,9.54581572176763));
#13492=CARTESIAN_POINT('Ctrl Pts',(6.67951438762365,-1.21022942861895,9.54617986991202));
#13493=CARTESIAN_POINT('Ctrl Pts',(6.68563611988732,-1.20216138888012,9.54683246126748));
#13494=CARTESIAN_POINT('Ctrl Pts',(6.68834214992285,-1.19856986352876,9.54712136954119));
#13495=CARTESIAN_POINT('Ctrl Pts',(6.69426152553844,-1.19065796048385,9.5477543162887));
#13496=CARTESIAN_POINT('Ctrl Pts',(6.69746952979353,-1.18633371724526,9.54809798707632));
#13497=CARTESIAN_POINT('Ctrl Pts',(6.7066479246318,-1.17385639869053,9.54908329692072));
#13498=CARTESIAN_POINT('Ctrl Pts',(6.71257402455141,-1.16567073487496,9.54972197642747));
#13499=CARTESIAN_POINT('Ctrl Pts',(6.75519727277702,-1.10584372710711,9.55433689328225));
#13500=CARTESIAN_POINT('Ctrl Pts',(6.78948196929028,-1.05251959611752,9.55816542616727));
#13501=CARTESIAN_POINT('Ctrl Pts',(6.88917882007176,-0.879902704455365,
9.56998592505028));
#13502=CARTESIAN_POINT('Ctrl Pts',(6.94496842010109,-0.755509949121724,
9.57771181580295));
#13503=CARTESIAN_POINT('Ctrl Pts',(7.00455075706617,-0.575371357012546,
9.58889908402287));
#13504=CARTESIAN_POINT('Ctrl Pts',(7.01935974925831,-0.523679768541553,
9.59210576573021));
#13505=CARTESIAN_POINT('Ctrl Pts',(7.04095496221828,-0.434898150257322,
9.59765952352239));
#13506=CARTESIAN_POINT('Ctrl Pts',(7.04881069084071,-0.398098219727024,
9.59997453170923));
#13507=CARTESIAN_POINT('Ctrl Pts',(7.0580277373281,-0.348023590749774,9.60315218491388));
#13508=CARTESIAN_POINT('Ctrl Pts',(7.06030379627913,-0.334923801939445,
9.60398598233022));
#13509=CARTESIAN_POINT('Ctrl Pts',(7.06383891523775,-0.313297768495138,
9.60536701102355));
#13510=CARTESIAN_POINT('Ctrl Pts',(7.06517400136076,-0.304784243023742,
9.60591183502028));
#13511=CARTESIAN_POINT('Ctrl Pts',(7.06759305366699,-0.288677283330814,
9.60694489277299));
#13512=CARTESIAN_POINT('Ctrl Pts',(7.06868847149326,-0.281085706829267,
9.60743275570657));
#13513=CARTESIAN_POINT('Ctrl Pts',(7.07083142104456,-0.265603198143267,
9.60842974767316));
#13514=CARTESIAN_POINT('Ctrl Pts',(7.07187555637616,-0.257711943088819,
9.60893897416393));
#13515=CARTESIAN_POINT('Ctrl Pts',(7.07418210140739,-0.239439374524609,
9.61012067163815));
#13516=CARTESIAN_POINT('Ctrl Pts',(7.07541015104722,-0.229054034506356,
9.61079420626002));
#13517=CARTESIAN_POINT('Ctrl Pts',(7.07947028174991,-0.192238192817203,
9.61318886685787));
#13518=CARTESIAN_POINT('Ctrl Pts',(7.08185555676161,-0.165762213074701,
9.61492377101967));
#13519=CARTESIAN_POINT('Ctrl Pts',(7.08698906719848,-0.0924029772202507,
9.61976789925707));
#13520=CARTESIAN_POINT('Ctrl Pts',(7.08861168291996,-0.0454612198587802,
9.62290974847365));
#13521=CARTESIAN_POINT('Ctrl Pts',(7.08857659854753,0.00149056180381668,
9.62609269279555));
#13522=CARTESIAN_POINT('Origin',(5.09382715545311,0.,-6.77268258743872));
#13523=CARTESIAN_POINT('',(7.08857715545311,-1.10669651073376E-10,10.5860251696757));
#13524=CARTESIAN_POINT('',(7.08881171743497,0.000532106016453122,10.4273173692856));
#13525=CARTESIAN_POINT('',(7.08857715545311,8.3550772080578E-14,-6.77268258743872));
#13526=CARTESIAN_POINT('Ctrl Pts',(7.08857715545311,-1.10669651073376E-10,
10.5860251696757));
#13527=CARTESIAN_POINT('Ctrl Pts',(7.08857715545308,-0.000599462547748238,
10.5859836762134));
#13528=CARTESIAN_POINT('Ctrl Pts',(7.0885768852439,-0.00119893046783767,
10.5859421786901));
#13529=CARTESIAN_POINT('Ctrl Pts',(7.08855819975973,-0.0219244591617089,
10.5845073491028));
#13530=CARTESIAN_POINT('Ctrl Pts',(7.08823546281962,-0.0420488502924382,
10.5831099857508));
#13531=CARTESIAN_POINT('Ctrl Pts',(7.08334007563174,-0.199056514380295,
10.5721835474355));
#13532=CARTESIAN_POINT('Ctrl Pts',(7.06498482681452,-0.335153859351847,
10.5625376395421));
#13533=CARTESIAN_POINT('Ctrl Pts',(7.02925382487065,-0.483097059662853,
10.5524634367512));
#13534=CARTESIAN_POINT('Ctrl Pts',(7.02551172804868,-0.497849281578507,
10.5514638891355));
#13535=CARTESIAN_POINT('Ctrl Pts',(7.02008491108987,-0.518260007798101,
10.5500892621842));
#13536=CARTESIAN_POINT('Ctrl Pts',(7.01854347556669,-0.523955595490136,
10.5497065780188));
#13537=CARTESIAN_POINT('Ctrl Pts',(7.01584851510462,-0.533741052855737,
10.5490507530661));
#13538=CARTESIAN_POINT('Ctrl Pts',(7.01470716270303,-0.537834191021118,
10.5487769292742));
#13539=CARTESIAN_POINT('Ctrl Pts',(7.01228918015534,-0.546399719620556,
10.5482050037561));
#13540=CARTESIAN_POINT('Ctrl Pts',(7.0110099759631,-0.550871334485474,10.5479070620912));
#13541=CARTESIAN_POINT('Ctrl Pts',(7.00784179232394,-0.561801398355937,
10.5471802526425));
#13542=CARTESIAN_POINT('Ctrl Pts',(7.00593572802216,-0.568254917424667,
10.5467523627501));
#13543=CARTESIAN_POINT('Ctrl Pts',(6.99892427357803,-0.591559419580452,
10.5452112931866));
#13544=CARTESIAN_POINT('Ctrl Pts',(6.9936283156223,-0.608352840223046,10.5441085519588));
#13545=CARTESIAN_POINT('Ctrl Pts',(6.97984412034227,-0.650125727974056,
10.5413798891469));
#13546=CARTESIAN_POINT('Ctrl Pts',(6.97108123491948,-0.675011636705886,
10.5397672521843));
#13547=CARTESIAN_POINT('Ctrl Pts',(6.93081162175451,-0.782517335977318,
10.5328278033662));
#13548=CARTESIAN_POINT('Ctrl Pts',(6.8943230200319,-0.863169943455942,10.5276889224015));
#13549=CARTESIAN_POINT('Ctrl Pts',(6.78401041632274,-1.06931865939343,10.514113730496));
#13550=CARTESIAN_POINT('Ctrl Pts',(6.70162343553738,-1.18959951639321,10.5056959185175));
#13551=CARTESIAN_POINT('Ctrl Pts',(6.59069502250191,-1.31872395567599,10.4952195192943));
#13552=CARTESIAN_POINT('Ctrl Pts',(6.57413520152104,-1.33728616469576,10.4936754518274));
#13553=CARTESIAN_POINT('Ctrl Pts',(6.5505292075649,-1.36277071357071,10.4914988814599));
#13554=CARTESIAN_POINT('Ctrl Pts',(6.54377174707401,-1.3699582336865,10.4908785244618));
#13555=CARTESIAN_POINT('Ctrl Pts',(6.53129710083977,-1.38303110480649,10.4897380531767));
#13556=CARTESIAN_POINT('Ctrl Pts',(6.52559635816397,-1.38893190173582,10.4892186505209));
#13557=CARTESIAN_POINT('Ctrl Pts',(6.51396563492926,-1.40082308260004,10.4881624373525));
#13558=CARTESIAN_POINT('Ctrl Pts',(6.5080337692579,-1.40681138022494,10.4876255501408));
#13559=CARTESIAN_POINT('Ctrl Pts',(6.49327891701845,-1.42151897575238,10.4862944045453));
#13560=CARTESIAN_POINT('Ctrl Pts',(6.48441230680191,-1.4301938178947,10.4854982251227));
#13561=CARTESIAN_POINT('Ctrl Pts',(6.45081511868682,-1.46245656496623,10.4824948176625));
#13562=CARTESIAN_POINT('Ctrl Pts',(6.42556180116407,-1.48548918950875,10.4802641400281));
#13563=CARTESIAN_POINT('Ctrl Pts',(6.36051180438649,-1.54182663092727,10.4745806688895));
#13564=CARTESIAN_POINT('Ctrl Pts',(6.31998581935925,-1.57424697616775,10.4710953775931));
#13565=CARTESIAN_POINT('Ctrl Pts',(6.18634617389968,-1.67286402788076,10.4597848540869));
#13566=CARTESIAN_POINT('Ctrl Pts',(6.088797928418,-1.73265731439188,10.4517835429541));
#13567=CARTESIAN_POINT('Ctrl Pts',(5.90555252806303,-1.82437940646711,10.4375350110504));
#13568=CARTESIAN_POINT('Ctrl Pts',(5.82173872983681,-1.85941036416094,10.4312865435898));
#13569=CARTESIAN_POINT('Ctrl Pts',(5.72545309321104,-1.89214063457353,10.424602328379));
#13570=CARTESIAN_POINT('Ctrl Pts',(5.71505478882372,-1.89558005548044,10.4238868000604));
#13571=CARTESIAN_POINT('Ctrl Pts',(5.69926636998255,-1.90065847698566,10.4228104791935));
#13572=CARTESIAN_POINT('Ctrl Pts',(5.69389697131518,-1.90236050910386,10.4224462005224));
#13573=CARTESIAN_POINT('Ctrl Pts',(5.68422791060329,-1.90538046943463,10.4217934722072));
#13574=CARTESIAN_POINT('Ctrl Pts',(5.67993095717825,-1.90670661607181,10.4215045565843));
#13575=CARTESIAN_POINT('Ctrl Pts',(5.6704809477854,-1.90958815915744,10.4208717079793));
#13576=CARTESIAN_POINT('Ctrl Pts',(5.66532607316748,-1.91113723277385,10.4205281418899));
#13577=CARTESIAN_POINT('Ctrl Pts',(5.65048310137547,-1.91553221751809,10.4195434346326));
#13578=CARTESIAN_POINT('Ctrl Pts',(5.64077941639249,-1.91832550752721,10.4189052473956));
#13579=CARTESIAN_POINT('Ctrl Pts',(5.57026570396313,-1.93804493492006,10.414305236726));
#13580=CARTESIAN_POINT('Ctrl Pts',(5.50869727104413,-1.95215172651041,10.4104900343397));
#13581=CARTESIAN_POINT('Ctrl Pts',(5.31807612803448,-1.98639880059593,10.3990037688106));
#13582=CARTESIAN_POINT('Ctrl Pts',(5.18763636419986,-1.99681505598292,10.3915750368805));
#13583=CARTESIAN_POINT('Ctrl Pts',(4.96779737679195,-1.99276778877225,10.3786422444231));
#13584=CARTESIAN_POINT('Ctrl Pts',(4.87870666721918,-1.98512650068646,10.3732908215123));
#13585=CARTESIAN_POINT('Ctrl Pts',(4.77494550999999,-1.96915912272347,10.3667756169436));
#13586=CARTESIAN_POINT('Ctrl Pts',(4.75948544460175,-1.966593184419,10.3657976005076));
#13587=CARTESIAN_POINT('Ctrl Pts',(4.73416024706406,-1.96208265408815,10.364182816774));
#13588=CARTESIAN_POINT('Ctrl Pts',(4.72427655714809,-1.96024513156493,10.3635494267183));
#13589=CARTESIAN_POINT('Ctrl Pts',(4.70651568697519,-1.95680402814337,10.3624053092976));
#13590=CARTESIAN_POINT('Ctrl Pts',(4.69863346171493,-1.95522738307424,10.3618954458368));
#13591=CARTESIAN_POINT('Ctrl Pts',(4.68183014341675,-1.95176053381556,10.3608039202311));
#13592=CARTESIAN_POINT('Ctrl Pts',(4.67291207741406,-1.9498567157173,10.3602218353381));
#13593=CARTESIAN_POINT('Ctrl Pts',(4.64878576231143,-1.94453302974595,10.3586394145476));
#13594=CARTESIAN_POINT('Ctrl Pts',(4.63360428940466,-1.94099599076064,10.3576353675814));
#13595=CARTESIAN_POINT('Ctrl Pts',(4.55305855206054,-1.92123205814174,10.3522628593987));
#13596=CARTESIAN_POINT('Ctrl Pts',(4.48851282294736,-1.90188225513687,10.3477952518183));
#13597=CARTESIAN_POINT('Ctrl Pts',(4.27204264495189,-1.82485126251408,10.3322480883833));
#13598=CARTESIAN_POINT('Ctrl Pts',(4.12624001382956,-1.75190665899648,10.3207397776508));
#13599=CARTESIAN_POINT('Ctrl Pts',(3.94415329151834,-1.6310817529194,10.3057369744724));
#13600=CARTESIAN_POINT('Ctrl Pts',(3.89871244618756,-1.59808627780061,10.3019400651605));
#13601=CARTESIAN_POINT('Ctrl Pts',(3.84741278736068,-1.55742278396653,10.2976432502069));
#13602=CARTESIAN_POINT('Ctrl Pts',(3.84014619881516,-1.55157937985299,10.2970343695622));
#13603=CARTESIAN_POINT('Ctrl Pts',(3.82844605819217,-1.54203488533367,10.2960539722246));
#13604=CARTESIAN_POINT('Ctrl Pts',(3.82398723351944,-1.53836519837608,10.2956803460877));
#13605=CARTESIAN_POINT('Ctrl Pts',(3.81607769436862,-1.53179769561979,10.2950176558302));
#13606=CARTESIAN_POINT('Ctrl Pts',(3.81262080356292,-1.52890750238688,10.2947280603738));
#13607=CARTESIAN_POINT('Ctrl Pts',(3.80514072526564,-1.52261046820306,10.2941015196967));
#13608=CARTESIAN_POINT('Ctrl Pts',(3.80112124224428,-1.5191993867589,10.2937648881957));
#13609=CARTESIAN_POINT('Ctrl Pts',(3.78983661918175,-1.50954562530997,10.2928197744973));
#13610=CARTESIAN_POINT('Ctrl Pts',(3.78260273786755,-1.50326639321613,10.2922138880703));
#13611=CARTESIAN_POINT('Ctrl Pts',(3.73748817822398,-1.46353212683689,10.2884329604784));
#13612=CARTESIAN_POINT('Ctrl Pts',(3.70084168171641,-1.42869665312083,10.2853514131281));
#13613=CARTESIAN_POINT('Ctrl Pts',(3.59549091598594,-1.32063978636248,10.2763178372346));
#13614=CARTESIAN_POINT('Ctrl Pts',(3.53094625167718,-1.24358622921299,10.27053801495));
#13615=CARTESIAN_POINT('Ctrl Pts',(3.395575430884,-1.05470108000084,10.2570342308051));
#13616=CARTESIAN_POINT('Ctrl Pts',(3.3295289033972,-0.940052350042298,10.249288977798));
#13617=CARTESIAN_POINT('Ctrl Pts',(3.26863874556675,-0.804970149263604,
10.2400999944944));
#13618=CARTESIAN_POINT('Ctrl Pts',(3.26216573500036,-0.790130425711512,
10.2390901648597));
#13619=CARTESIAN_POINT('Ctrl Pts',(3.25190633737254,-0.765806441943793,
10.237433555207));
#13620=CARTESIAN_POINT('Ctrl Pts',(3.24801080081811,-0.756368815693512,
10.2367904618385));
#13621=CARTESIAN_POINT('Ctrl Pts',(3.24117241336094,-0.739434127717005,
10.23563572281));
#13622=CARTESIAN_POINT('Ctrl Pts',(3.23820217058637,-0.731948314481599,
10.235125009734));
#13623=CARTESIAN_POINT('Ctrl Pts',(3.23200146009965,-0.716040506210221,
10.2340390415917));
#13624=CARTESIAN_POINT('Ctrl Pts',(3.22878263297337,-0.707614196571379,
10.2334634113715));
#13625=CARTESIAN_POINT('Ctrl Pts',(3.22031567293655,-0.684990076442046,
10.2319166710647));
#13626=CARTESIAN_POINT('Ctrl Pts',(3.21517189284533,-0.670754100506691,
10.2309421303004));
#13627=CARTESIAN_POINT('Ctrl Pts',(3.19013613469209,-0.598917014140809,
10.2260170331588));
#13628=CARTESIAN_POINT('Ctrl Pts',(3.17273093725686,-0.540489689512963,
10.2219860602655));
#13629=CARTESIAN_POINT('Ctrl Pts',(3.12687280475239,-0.356071155971735,
10.2091794492502));
#13630=CARTESIAN_POINT('Ctrl Pts',(3.10795787543648,-0.2280622679266,10.2001489053877));
#13631=CARTESIAN_POINT('Ctrl Pts',(3.09680021821498,-0.00384584750200338,
10.1845257738886));
#13632=CARTESIAN_POINT('Ctrl Pts',(3.09890095585723,0.0916794254478449,
10.1779397834552));
#13633=CARTESIAN_POINT('Ctrl Pts',(3.10885811519948,0.197599038056236,10.1709473268837));
#13634=CARTESIAN_POINT('Ctrl Pts',(3.10997277717449,0.208492899953273,10.1702319064362));
#13635=CARTESIAN_POINT('Ctrl Pts',(3.11179654097423,0.224975393944017,10.1691557156769));
#13636=CARTESIAN_POINT('Ctrl Pts',(3.11243967559041,0.230570902617754,10.1687914604506));
#13637=CARTESIAN_POINT('Ctrl Pts',(3.11363891310289,0.240628987555381,10.1681387570443));
#13638=CARTESIAN_POINT('Ctrl Pts',(3.11418641146809,0.245092453436738,10.1678498430485));
#13639=CARTESIAN_POINT('Ctrl Pts',(3.11542243387575,0.254894673469399,10.1672169778063));
#13640=CARTESIAN_POINT('Ctrl Pts',(3.11611747397427,0.26023250055568,10.1668733935923));
#13641=CARTESIAN_POINT('Ctrl Pts',(3.11817859434596,0.275576321791976,10.1658885819915));
#13642=CARTESIAN_POINT('Ctrl Pts',(3.11959908656849,0.285575013376463,10.1652503095084));
#13643=CARTESIAN_POINT('Ctrl Pts',(3.13045408936712,0.358026663959927,10.1606477238445));
#13644=CARTESIAN_POINT('Ctrl Pts',(3.14277522590672,0.420017827779554,10.1568302185709));
#13645=CARTESIAN_POINT('Ctrl Pts',(3.18957155994404,0.608224480438732,10.1453285939656));
#13646=CARTESIAN_POINT('Ctrl Pts',(3.23352594698046,0.731716165531569,10.1378875836846));
#13647=CARTESIAN_POINT('Ctrl Pts',(3.3272109076008,0.930607053516934,10.1249548485714));
#13648=CARTESIAN_POINT('Ctrl Pts',(3.3705204314355,1.00855019360554,10.1196177254241));
#13649=CARTESIAN_POINT('Ctrl Pts',(3.42739547724703,1.09648453976341,10.1131184577155));
#13650=CARTESIAN_POINT('Ctrl Pts',(3.43605619823787,1.10953518002995,10.1121409708667));
#13651=CARTESIAN_POINT('Ctrl Pts',(3.4505250831585,1.13079037534133,10.1105268838046));
#13652=CARTESIAN_POINT('Ctrl Pts',(3.45624327171693,1.13905557001066,10.1098936557819));
#13653=CARTESIAN_POINT('Ctrl Pts',(3.46664672929416,1.15385269219551,10.1087497138347));
#13654=CARTESIAN_POINT('Ctrl Pts',(3.47130951288325,1.16040022019669,10.1082398626659));
#13655=CARTESIAN_POINT('Ctrl Pts',(3.48134730724134,1.1743166057018,10.1071482355477));
#13656=CARTESIAN_POINT('Ctrl Pts',(3.48673352435178,1.18167711649526,10.1065660360181));
#13657=CARTESIAN_POINT('Ctrl Pts',(3.50146614169614,1.20152286590383,10.1049829812778));
#13658=CARTESIAN_POINT('Ctrl Pts',(3.51090864008498,1.21393564339,10.1039784099382));
#13659=CARTESIAN_POINT('Ctrl Pts',(3.56197123760016,1.27945189959197,10.0985974386307));
#13660=CARTESIAN_POINT('Ctrl Pts',(3.60611560835696,1.33052332176757,10.0941215172144));
#13661=CARTESIAN_POINT('Ctrl Pts',(3.76562505819221,1.49718138558852,10.0785107287734));
#13662=CARTESIAN_POINT('Ctrl Pts',(3.89253845144535,1.60080236122784,10.066942226672));
#13663=CARTESIAN_POINT('Ctrl Pts',(4.07738078135029,1.71724129427331,10.0519513458941));
#13664=CARTESIAN_POINT('Ctrl Pts',(4.12534295215322,1.74474079303491,10.0482150906697));
#13665=CARTESIAN_POINT('Ctrl Pts',(4.1826324038277,1.77449653701363,10.0439780042499));
#13666=CARTESIAN_POINT('Ctrl Pts',(4.19090519114034,1.77872026174765,10.0433715082488));
#13667=CARTESIAN_POINT('Ctrl Pts',(4.20435903567263,1.78547115585104,10.0423941842037));
#13668=CARTESIAN_POINT('Ctrl Pts',(4.2095219622558,1.7880338676253,10.0420212676046));
#13669=CARTESIAN_POINT('Ctrl Pts',(4.21873992210693,1.79255967597386,10.0413593446132));
#13670=CARTESIAN_POINT('Ctrl Pts',(4.2227905638387,1.79453144729192,10.0410698118255));
#13671=CARTESIAN_POINT('Ctrl Pts',(4.23160272861058,1.79878416526217,10.040442842516));
#13672=CARTESIAN_POINT('Ctrl Pts',(4.23636663497285,1.80105993592911,10.0401057235068));
#13673=CARTESIAN_POINT('Ctrl Pts',(4.24983169074333,1.80742680706651,10.0391578458821));
#13674=CARTESIAN_POINT('Ctrl Pts',(4.25855360321885,1.81147401556139,10.0385497073387));
#13675=CARTESIAN_POINT('Ctrl Pts',(4.3139801319694,1.83670801783921,10.0347198434615));
#13676=CARTESIAN_POINT('Ctrl Pts',(4.36146226365271,1.85615203459918,10.0315944346581));
#13677=CARTESIAN_POINT('Ctrl Pts',(4.55390681186152,1.9264214722359,10.0193383691277));
#13678=CARTESIAN_POINT('Ctrl Pts',(4.70377437515435,1.96226359983741,10.0106655790503));
#13679=CARTESIAN_POINT('Ctrl Pts',(4.93543258137789,1.99004880409893,9.99687928098526));
#13680=CARTESIAN_POINT('Ctrl Pts',(5.0150763202738,1.99478800668835,9.99208099290881));
#13681=CARTESIAN_POINT('Ctrl Pts',(5.11008104609107,1.99474243243903,9.98618193123487));
#13682=CARTESIAN_POINT('Ctrl Pts',(5.12537711085488,1.99455913443252,9.98522690014019));
#13683=CARTESIAN_POINT('Ctrl Pts',(5.15060532600748,1.99396654493551,9.98364237902414));
#13684=CARTESIAN_POINT('Ctrl Pts',(5.16053939128895,1.99365890132386,9.98301605018612));
#13685=CARTESIAN_POINT('Ctrl Pts',(5.17849391892104,1.99296853223438,9.98187953720926));
#13686=CARTESIAN_POINT('Ctrl Pts',(5.18651520419292,1.99261159132031,9.9813701669821));
#13687=CARTESIAN_POINT('Ctrl Pts',(5.20372064211897,1.99174184917191,9.98027399464174));
#13688=CARTESIAN_POINT('Ctrl Pts',(5.21290381156008,1.99121393061263,9.97968673241593));
#13689=CARTESIAN_POINT('Ctrl Pts',(5.23800135396251,1.98959689706702,9.97807558527741));
#13690=CARTESIAN_POINT('Ctrl Pts',(5.25390656007519,1.98838038919043,9.9770477567756));
#13691=CARTESIAN_POINT('Ctrl Pts',(5.34270810250086,1.98051605385441,9.97126993128384));
#13692=CARTESIAN_POINT('Ctrl Pts',(5.41520180019137,1.97005118601866,9.96640193318113));
#13693=CARTESIAN_POINT('Ctrl Pts',(5.58301898027906,1.9363163957845,9.95477916896341));
#13694=CARTESIAN_POINT('Ctrl Pts',(5.67752771218157,1.90995304332527,9.94795560492661));
#13695=CARTESIAN_POINT('Ctrl Pts',(5.86810284474545,1.84132065702192,9.93383479326349));
#13696=CARTESIAN_POINT('Ctrl Pts',(5.96356794133179,1.79819906362994,9.92655841622439));
#13697=CARTESIAN_POINT('Ctrl Pts',(6.06945905914812,1.73995232816911,9.91854710021814));
#13698=CARTESIAN_POINT('Ctrl Pts',(6.08360392465455,1.73194506360236,9.9174784622305));
#13699=CARTESIAN_POINT('Ctrl Pts',(6.10346737371326,1.72037772381891,9.91598160774956));
#13700=CARTESIAN_POINT('Ctrl Pts',(6.10926779321026,1.7169604530348,9.91554497127354));
#13701=CARTESIAN_POINT('Ctrl Pts',(6.11890370288825,1.71121762234335,9.91482053516186));
#13702=CARTESIAN_POINT('Ctrl Pts',(6.1227488084779,1.70890839787518,9.91453170365837));
#13703=CARTESIAN_POINT('Ctrl Pts',(6.13059989898833,1.70415722594928,9.91394251344165));
#13704=CARTESIAN_POINT('Ctrl Pts',(6.13460511205222,1.70171408252216,9.91364223526679));
#13705=CARTESIAN_POINT('Ctrl Pts',(6.14468430313437,1.69551697184758,9.91288722902877));
#13706=CARTESIAN_POINT('Ctrl Pts',(6.1507468738196,1.69174444266313,9.91243369503725));
#13707=CARTESIAN_POINT('Ctrl Pts',(6.16390250842044,1.68345982057725,9.91145054395757));
#13708=CARTESIAN_POINT('Ctrl Pts',(6.17098760457852,1.67893525812927,9.91092170137893));
#13709=CARTESIAN_POINT('Ctrl Pts',(6.19139445401717,1.66572103191961,9.90939972331708));
#13710=CARTESIAN_POINT('Ctrl Pts',(6.204641459335,1.6569164575297,9.90841325528953));
#13711=CARTESIAN_POINT('Ctrl Pts',(6.25053041079244,1.6256187911397,9.9049961044636));
#13712=CARTESIAN_POINT('Ctrl Pts',(6.2826076690896,1.60231087895737,9.90260751065806));
#13713=CARTESIAN_POINT('Ctrl Pts',(6.38771528200104,1.52104254941276,9.89470458506133));
#13714=CARTESIAN_POINT('Ctrl Pts',(6.45737568526177,1.45892221067634,9.88933392394672));
#13715=CARTESIAN_POINT('Ctrl Pts',(6.6133136861744,1.29890064862328,9.87634709284605));
#13716=CARTESIAN_POINT('Ctrl Pts',(6.69482688753028,1.19698607437713,9.86870042755989));
#13717=CARTESIAN_POINT('Ctrl Pts',(6.77466216495409,1.07428291859378,9.85962216126105));
#13718=CARTESIAN_POINT('Ctrl Pts',(6.78333298281527,1.06059424551384,9.85861148788484));
#13719=CARTESIAN_POINT('Ctrl Pts',(6.79719604296018,1.03810708711837,9.85695376984846));
#13720=CARTESIAN_POINT('Ctrl Pts',(6.80248926312967,1.02937150088087,9.85631042020696));
#13721=CARTESIAN_POINT('Ctrl Pts',(6.8118358479494,1.01367576780172,9.85515539809639));
#13722=CARTESIAN_POINT('Ctrl Pts',(6.81591461553315,1.00673095038384,9.85464466002542));
#13723=CARTESIAN_POINT('Ctrl Pts',(6.82447082143923,0.991958357690129,9.85355882648744));
#13724=CARTESIAN_POINT('Ctrl Pts',(6.82893744815606,0.984124560092876,9.85298335706967));
#13725=CARTESIAN_POINT('Ctrl Pts',(6.84075334344385,0.963070731518586,9.85143750457792));
#13726=CARTESIAN_POINT('Ctrl Pts',(6.8480055059105,0.949797154214314,9.85046369768773));
#13727=CARTESIAN_POINT('Ctrl Pts',(6.88364373198603,0.882768120150708,9.845549061164));
#13728=CARTESIAN_POINT('Ctrl Pts',(6.90971033082473,0.827822400030444,9.84152822726493));
#13729=CARTESIAN_POINT('Ctrl Pts',(7.00196410874102,0.607951264074163,9.82546103938766));
#13730=CARTESIAN_POINT('Ctrl Pts',(7.04849753441028,0.435707167263862,9.81283344067696));
#13731=CARTESIAN_POINT('Ctrl Pts',(7.07540183278938,0.230731212823433,9.79870074335504));
#13732=CARTESIAN_POINT('Ctrl Pts',(7.07855834208674,0.201785468863893,9.79672771518192));
#13733=CARTESIAN_POINT('Ctrl Pts',(7.0831453897689,0.149026805318393,9.79318415203214));
#13734=CARTESIAN_POINT('Ctrl Pts',(7.08478464020475,0.125237536219724,9.79160570920069));
#13735=CARTESIAN_POINT('Ctrl Pts',(7.08639479774754,0.0936106327978812,
9.7895378267005));
#13736=CARTESIAN_POINT('Ctrl Pts',(7.08674659782671,0.0857954589777864,
9.78902932055115));
#13737=CARTESIAN_POINT('Ctrl Pts',(7.08724338865359,0.07309684294638,9.78820730907328));
#13738=CARTESIAN_POINT('Ctrl Pts',(7.08741642780105,0.0682146733619648,
9.78789229300434));
#13739=CARTESIAN_POINT('Ctrl Pts',(7.0877073502051,0.0590561714255483,9.78730332351803));
#13740=CARTESIAN_POINT('Ctrl Pts',(7.08782941431966,0.054780054595996,9.78702914421586));
#13741=CARTESIAN_POINT('Ctrl Pts',(7.08805314356808,0.0459462026499021,
9.78646434933058));
#13742=CARTESIAN_POINT('Ctrl Pts',(7.08815294246162,0.0413884219076879,
9.78617383625334));
#13743=CARTESIAN_POINT('Ctrl Pts',(7.0883496707764,0.0307353165076802,9.78549680352272));
#13744=CARTESIAN_POINT('Ctrl Pts',(7.08843428662043,0.0246397717790206,
9.78511094297792));
#13745=CARTESIAN_POINT('Ctrl Pts',(7.08854690723099,0.0125257642969657,
9.78434696682734));
#13746=CARTESIAN_POINT('Ctrl Pts',(7.08857562044335,0.00650738875274101,
9.7839688201241));
#13747=CARTESIAN_POINT('Ctrl Pts',(7.08857709553963,0.000488901638750699,
9.78359198969069));
#13748=CARTESIAN_POINT('Ctrl Pts',(7.08857665886015,0.00140753592649714,
9.62731741260996));
#13749=CARTESIAN_POINT('Ctrl Pts',(7.08852025530264,0.0813422404025034,
9.63240191524386));
#13750=CARTESIAN_POINT('Ctrl Pts',(7.08365504861875,0.161085982574378,9.63748641787775));
#13751=CARTESIAN_POINT('Ctrl Pts',(7.07407361416448,0.240107320298838,9.64257092051165));
#13752=CARTESIAN_POINT('Ctrl Pts',(7.0644056661666,0.319842164542561,9.64770133259078));
#13753=CARTESIAN_POINT('Ctrl Pts',(7.04993604781898,0.398841308736947,9.6528317446699));
#13754=CARTESIAN_POINT('Ctrl Pts',(7.03080957818391,0.476578069713561,9.65796215674903));
#13755=CARTESIAN_POINT('Ctrl Pts',(7.0133888038839,0.547382279461962,9.66263503954453));
#13756=CARTESIAN_POINT('Ctrl Pts',(6.99210541276568,0.617139371892782,9.66730792234004));
#13757=CARTESIAN_POINT('Ctrl Pts',(6.96710304201831,0.685467005269678,9.67198080513555));
#13758=CARTESIAN_POINT('Ctrl Pts',(6.94326378476616,0.75061602837474,9.67643630482383));
#13759=CARTESIAN_POINT('Ctrl Pts',(6.91597500802296,0.814647922360064,9.68089180451211));
#13760=CARTESIAN_POINT('Ctrl Pts',(6.8853617690878,0.877172326654685,9.68534730420039));
#13761=CARTESIAN_POINT('Ctrl Pts',(6.85479430590389,0.939603238666971,9.68979614161273));
#13762=CARTESIAN_POINT('Ctrl Pts',(6.82091246049086,1.00053069921662,9.69424497902506));
#13763=CARTESIAN_POINT('Ctrl Pts',(6.78389005025252,1.05958245272478,9.69869381643739));
#13764=CARTESIAN_POINT('Ctrl Pts',(6.7469109726107,1.11856508956029,9.70313744674205));
#13765=CARTESIAN_POINT('Ctrl Pts',(6.70679888962395,1.17567596732585,9.7075810770467));
#13766=CARTESIAN_POINT('Ctrl Pts',(6.66377357393471,1.2305672698381,9.71202470735136));
#13767=CARTESIAN_POINT('Ctrl Pts',(6.62077516153372,1.28542424938235,9.7164655590996));
#13768=CARTESIAN_POINT('Ctrl Pts',(6.57486743131534,1.33806402288491,9.72090641084784));
#13769=CARTESIAN_POINT('Ctrl Pts',(6.52631264525958,1.38816889606198,9.72534726259608));
#13770=CARTESIAN_POINT('Ctrl Pts',(6.47777175274261,1.43825943215601,9.72978684363239));
#13771=CARTESIAN_POINT('Ctrl Pts',(6.42658564834507,1.48581615680537,9.73422642466869));
#13772=CARTESIAN_POINT('Ctrl Pts',(6.37305474201621,1.53055687391092,9.738666005705));
#13773=CARTESIAN_POINT('Ctrl Pts',(6.31952099876136,1.57529996209724,9.74310582202152));
#13774=CARTESIAN_POINT('Ctrl Pts',(6.26364258375581,1.61722643461298,9.74754563833803));
#13775=CARTESIAN_POINT('Ctrl Pts',(6.20575302226661,1.65609432980463,9.75198545465455));
#13776=CARTESIAN_POINT('Ctrl Pts',(6.14780235396479,1.69500325300077,9.75642995753315));
#13777=CARTESIAN_POINT('Ctrl Pts',(6.08783670902331,1.7308468818767,9.76087446041174));
#13778=CARTESIAN_POINT('Ctrl Pts',(6.02621782555706,1.76342711808657,9.76531896329034));
#13779=CARTESIAN_POINT('Ctrl Pts',(5.9645627950711,1.79602646659407,9.76976607341405));
#13780=CARTESIAN_POINT('Ctrl Pts',(5.90125303967262,1.82535840636816,9.77421318353777));
#13781=CARTESIAN_POINT('Ctrl Pts',(5.83667154955317,1.85127247282892,9.77866029366148));
#13782=CARTESIAN_POINT('Ctrl Pts',(5.77197855925583,1.8772312800198,9.78311508173702));
#13783=CARTESIAN_POINT('Ctrl Pts',(5.70600991434269,1.89976027706512,9.78756986981256));
#13784=CARTESIAN_POINT('Ctrl Pts',(5.63916428794348,1.91875870667137,9.79202465788809));
#13785=CARTESIAN_POINT('Ctrl Pts',(5.60523510120037,1.92840183967287,9.79428579814001));
#13786=CARTESIAN_POINT('Ctrl Pts',(5.57108014905197,1.93713619981271,9.79654693839193));
#13787=CARTESIAN_POINT('Ctrl Pts',(5.53675230609608,1.9449536944174,9.79880807864385));
#13788=CARTESIAN_POINT('Ctrl Pts',(5.46911046323752,1.96035780070738,9.80326357833248));
#13789=CARTESIAN_POINT('Ctrl Pts',(5.40053119820327,1.97225927914909,9.80771907802112));
#13790=CARTESIAN_POINT('Ctrl Pts',(5.33141014156992,1.98055090497766,9.81217457770975));
#13791=CARTESIAN_POINT('Ctrl Pts',(5.26239244114616,1.98883013239887,9.81662341512234));
#13792=CARTESIAN_POINT('Ctrl Pts',(5.19283503888196,1.9935101629964,9.82107225253493));
#13793=CARTESIAN_POINT('Ctrl Pts',(5.1231448738556,1.99453454066047,9.82552108994752));
#13794=CARTESIAN_POINT('Ctrl Pts',(5.05353627715152,1.99555771934951,9.82996472025228));
#13795=CARTESIAN_POINT('Ctrl Pts',(4.98379571311575,1.99293373624857,9.83440835055704));
#13796=CARTESIAN_POINT('Ctrl Pts',(4.91433458783194,1.98665799287868,9.8388519808618));
#13797=CARTESIAN_POINT('Ctrl Pts',(4.84491689587822,1.98038617366684,9.84329283261005));
#13798=CARTESIAN_POINT('Ctrl Pts',(4.7757787821183,1.97046716802976,9.8477336843583));
#13799=CARTESIAN_POINT('Ctrl Pts',(4.70732946599528,1.95694841489084,9.85217453610656));
#13800=CARTESIAN_POINT('Ctrl Pts',(4.63889973606288,1.94343353002834,9.85661411714279));
#13801=CARTESIAN_POINT('Ctrl Pts',(4.57115889214703,1.92632103729661,9.86105369817902));
#13802=CARTESIAN_POINT('Ctrl Pts',(4.50450709454416,1.90570969150872,9.86549327921525));
#13803=CARTESIAN_POINT('Ctrl Pts',(4.43785176466142,1.88509725340158,9.8699330955316));
#13804=CARTESIAN_POINT('Ctrl Pts',(4.3722860622907,1.86098574094044,9.87437291184795));
#13805=CARTESIAN_POINT('Ctrl Pts',(4.30819437751614,1.83352357517732,9.8788127281643));
#13806=CARTESIAN_POINT('Ctrl Pts',(4.24403503912045,1.80603242102103,9.88325723104259));
#13807=CARTESIAN_POINT('Ctrl Pts',(4.18135327427906,1.7751837474656,9.88770173392088));
#13808=CARTESIAN_POINT('Ctrl Pts',(4.1205119920654,1.74117349945936,9.89214623679917));
#13809=CARTESIAN_POINT('Ctrl Pts',(4.05963501899147,1.7071433002791,9.8965933469225));
#13810=CARTESIAN_POINT('Ctrl Pts',(4.00060109148739,1.6699480959816,9.90104045704583));
#13811=CARTESIAN_POINT('Ctrl Pts',(3.94374468911479,1.62982756238848,9.90548756716917));
#13812=CARTESIAN_POINT('Ctrl Pts',(3.8867901239578,1.58963776054896,9.90994235524422));
#13813=CARTESIAN_POINT('Ctrl Pts',(3.83202097241562,1.54651285059152,9.91439714331927));
#13814=CARTESIAN_POINT('Ctrl Pts',(3.77973851683813,1.50073269184189,9.91885193139432));
#13815=CARTESIAN_POINT('Ctrl Pts',(3.75320123541932,1.47749581548026,9.92111307164687));
#13816=CARTESIAN_POINT('Ctrl Pts',(3.72730401706465,1.45357544997633,9.92337421189943));
#13817=CARTESIAN_POINT('Ctrl Pts',(3.70208239602652,1.42901157696802,9.92563535215199));
#13818=CARTESIAN_POINT('Ctrl Pts',(3.6523840522613,1.38060930325504,9.93009085187593));
#13819=CARTESIAN_POINT('Ctrl Pts',(3.60511609883124,1.32951623683033,9.93454635159989));
#13820=CARTESIAN_POINT('Ctrl Pts',(3.56058359273093,1.27600616764614,9.93900185132384));
#13821=CARTESIAN_POINT('Ctrl Pts',(3.51611767575858,1.22257611167379,9.9434506887719));
#13822=CARTESIAN_POINT('Ctrl Pts',(3.47437939805803,1.16673659927669,9.94789952621997));
#13823=CARTESIAN_POINT('Ctrl Pts',(3.43563735068529,1.10879850913684,9.95234836366803));
#13824=CARTESIAN_POINT('Ctrl Pts',(3.39694064864549,1.05092823219131,9.95679199400835));
#13825=CARTESIAN_POINT('Ctrl Pts',(3.36123348221421,0.990964660774739,9.96123562434866));
#13826=CARTESIAN_POINT('Ctrl Pts',(3.32874334356431,0.929250611787858,9.96567925468898));
#13827=CARTESIAN_POINT('Ctrl Pts',(3.29627352066493,0.867575151962949,9.97012010647281));
#13828=CARTESIAN_POINT('Ctrl Pts',(3.26701696225748,0.804151817862348,9.97456095825664));
#13829=CARTESIAN_POINT('Ctrl Pts',(3.24115629394578,0.73934987754221,9.97900181004047));
#13830=CARTESIAN_POINT('Ctrl Pts',(3.21530302544484,0.674566479747334,9.98344139111225));
#13831=CARTESIAN_POINT('Ctrl Pts',(3.19284389916565,0.608405712978014,9.98788097218403));
#13832=CARTESIAN_POINT('Ctrl Pts',(3.17391354398806,0.541257135760092,9.99232055325581));
#13833=CARTESIAN_POINT('Ctrl Pts',(3.15498218557738,0.474104999936243,9.99676036960763));
#13834=CARTESIAN_POINT('Ctrl Pts',(3.13958009994461,0.405965421204017,10.0012001859594));
#13835=CARTESIAN_POINT('Ctrl Pts',(3.12779165588568,0.337241718861464,10.0056400023113));
#13836=CARTESIAN_POINT('Ctrl Pts',(3.11599076823344,0.268445473459133,10.0100845052247));
#13837=CARTESIAN_POINT('Ctrl Pts',(3.10781121821081,0.199064356886703,10.0145290081381));
#13838=CARTESIAN_POINT('Ctrl Pts',(3.10328580844011,0.12950949128021,10.0189735110514));
#13839=CARTESIAN_POINT('Ctrl Pts',(3.09875774396275,0.0599138232328149,
10.0234206212097));
#13840=CARTESIAN_POINT('Ctrl Pts',(3.09788809245653,-0.00985530746950176,
10.027867731368));
#13841=CARTESIAN_POINT('Ctrl Pts',(3.1006574969992,-0.0793868699390318,
10.0323148415263));
#13842=CARTESIAN_POINT('Ctrl Pts',(3.10343168292841,-0.149038478892176,
10.0367696296357));
#13843=CARTESIAN_POINT('Ctrl Pts',(3.10985742085494,-0.218451213938643,
10.041224417745));
#13844=CARTESIAN_POINT('Ctrl Pts',(3.11986358019106,-0.287220065522337,
10.0456792058544));
#13845=CARTESIAN_POINT('Ctrl Pts',(3.12494245844923,-0.32212542865076,10.0479403457897));
#13846=CARTESIAN_POINT('Ctrl Pts',(3.13094295371157,-0.356865081974095,
10.050201485725));
#13847=CARTESIAN_POINT('Ctrl Pts',(3.13785082285443,-0.391387466347351,
10.0524626256602));
#13848=CARTESIAN_POINT('Ctrl Pts',(3.15146254500617,-0.459412655358127,
10.0569181253098));
#13849=CARTESIAN_POINT('Ctrl Pts',(3.16865391578513,-0.52686054247854,10.0613736249593));
#13850=CARTESIAN_POINT('Ctrl Pts',(3.18936095080603,-0.593326249088268,
10.0658291246088));
#13851=CARTESIAN_POINT('Ctrl Pts',(3.21003702274976,-0.659692570015737,
10.0702779619825));
#13852=CARTESIAN_POINT('Ctrl Pts',(3.23421818055781,-0.725079162137858,
10.0747267993562));
#13853=CARTESIAN_POINT('Ctrl Pts',(3.26178948698271,-0.789091594053275,
10.0791756367299));
#13854=CARTESIAN_POINT('Ctrl Pts',(3.28932852278481,-0.853029103111823,
10.0836192669962));
#13855=CARTESIAN_POINT('Ctrl Pts',(3.32024963353363,-0.915595199337671,
10.0880628972625));
#13856=CARTESIAN_POINT('Ctrl Pts',(3.35438873385719,-0.97641258696102,10.0925065275288));
#13857=CARTESIAN_POINT('Ctrl Pts',(3.3885064873532,-1.03719194609873,10.0969473792389));
#13858=CARTESIAN_POINT('Ctrl Pts',(3.42583799967954,-1.09622434027595,10.101388230949));
#13859=CARTESIAN_POINT('Ctrl Pts',(3.46617259490296,-1.15315575444963,10.1058290826591));
#13860=CARTESIAN_POINT('Ctrl Pts',(3.50649564872761,-1.21007087818703,10.1102686636576));
#13861=CARTESIAN_POINT('Ctrl Pts',(3.54981979684907,-1.26488581646807,10.114708244656));
#13862=CARTESIAN_POINT('Ctrl Pts',(3.59589124229518,-1.31727581112374,10.1191478256545));
#13863=CARTESIAN_POINT('Ctrl Pts',(3.64196512934875,-1.36966858224542,10.1235876419335));
#13864=CARTESIAN_POINT('Ctrl Pts',(3.69078627793172,-1.41963578886794,10.1280274582124));
#13865=CARTESIAN_POINT('Ctrl Pts',(3.74206202046107,-1.46688737888086,10.1324672744914));
#13866=CARTESIAN_POINT('Ctrl Pts',(3.79339188842568,-1.51418884653085,10.1369117773332));
#13867=CARTESIAN_POINT('Ctrl Pts',(3.84718116123485,-1.5587686441913,10.141356280175));
#13868=CARTESIAN_POINT('Ctrl Pts',(3.90310259156291,-1.60037576070387,10.1458007830168));
#13869=CARTESIAN_POINT('Ctrl Pts',(3.95905682666169,-1.64200728488823,10.1502478931041));
#13870=CARTESIAN_POINT('Ctrl Pts',(4.0171453014733,-1.68066238591739,10.1546950031914));
#13871=CARTESIAN_POINT('Ctrl Pts',(4.07701249234068,-1.71613388270833,10.1591421132787));
#13872=CARTESIAN_POINT('Ctrl Pts',(4.13698304414484,-1.75166662117578,10.1635969013187));
#13873=CARTESIAN_POINT('Ctrl Pts',(4.19873800863606,-1.78400455710301,10.1680516893588));
#13874=CARTESIAN_POINT('Ctrl Pts',(4.26189877303869,-1.81298723907074,10.1725064773989));
#13875=CARTESIAN_POINT('Ctrl Pts',(4.29395762001292,-1.82769813395768,10.1747676179888));
#13876=CARTESIAN_POINT('Ctrl Pts',(4.32637835074632,-1.84154538609442,10.1770287585786));
#13877=CARTESIAN_POINT('Ctrl Pts',(4.35910994638157,-1.85451292397603,10.1792898991685));
#13878=CARTESIAN_POINT('Ctrl Pts',(4.42360642854782,-1.88006501086606,10.183745398844));
#13879=CARTESIAN_POINT('Ctrl Pts',(4.48956417630287,-1.90229868475508,10.1882008985195));
#13880=CARTESIAN_POINT('Ctrl Pts',(4.5566085713,-1.9210475671728,10.192656398195));
#13881=CARTESIAN_POINT('Ctrl Pts',(4.62355271529725,-1.93976841452197,10.197105235594));
#13882=CARTESIAN_POINT('Ctrl Pts',(4.69157981419015,-1.95501468213493,10.2015540729929));
#13883=CARTESIAN_POINT('Ctrl Pts',(4.76029632158471,-1.96666843808484,10.2060029103919));
#13884=CARTESIAN_POINT('Ctrl Pts',(4.82893240025759,-1.97830855398333,10.2104465406825));
#13885=CARTESIAN_POINT('Ctrl Pts',(4.89825580476789,-1.98636442833082,10.214890170973));
#13886=CARTESIAN_POINT('Ctrl Pts',(4.96786065566025,-1.99076869661695,10.2193338012636));
#13887=CARTESIAN_POINT('Ctrl Pts',(5.03742198334651,-1.99517021095886,10.2237746529972));
#13888=CARTESIAN_POINT('Ctrl Pts',(5.1072639212017,-1.99592461815519,10.2282155047309));
#13889=CARTESIAN_POINT('Ctrl Pts',(5.17697480487905,-1.99301631475885,10.2326563564646));
#13890=CARTESIAN_POINT('Ctrl Pts',(5.24666574137353,-1.99010884354906,10.2370959374859));
#13891=CARTESIAN_POINT('Ctrl Pts',(5.31622520963413,-1.98354076279362,10.2415355185072));
#13892=CARTESIAN_POINT('Ctrl Pts',(5.38524266250854,-1.97334856645947,10.2459750995285));
#13893=CARTESIAN_POINT('Ctrl Pts',(5.45426377302825,-1.96315582998021,10.2504149158296));
#13894=CARTESIAN_POINT('Ctrl Pts',(5.5227423275696,-1.94933867047341,10.2548547321308));
#13895=CARTESIAN_POINT('Ctrl Pts',(5.590275780436,-1.93198507376548,10.2592945484319));
#13896=CARTESIAN_POINT('Ctrl Pts',(5.65788051996472,-1.91461315902499,10.2637390512946));
#13897=CARTESIAN_POINT('Ctrl Pts',(5.72453769198412,-1.89369747852418,10.2681835541573));
#13898=CARTESIAN_POINT('Ctrl Pts',(5.78985872320934,-1.86937626474362,10.27262805702));
#13899=CARTESIAN_POINT('Ctrl Pts',(5.85521807321282,-1.84504078359494,10.2770751671275));
#13900=CARTESIAN_POINT('Ctrl Pts',(5.91923927338325,-1.81729598738069,10.281522277235));
#13901=CARTESIAN_POINT('Ctrl Pts',(5.98155516904373,-1.78632766769886,10.2859693873425));
#13902=CARTESIAN_POINT('Ctrl Pts',(6.04397865332126,-1.75530588110218,10.2904241754015));
#13903=CARTESIAN_POINT('Ctrl Pts',(6.10469053029643,-1.72104970235199,10.2948789634605));
#13904=CARTESIAN_POINT('Ctrl Pts',(6.16335031735875,-1.68378970440117,10.2993337515196));
#13905=CARTESIAN_POINT('Ctrl Pts',(6.19312457637739,-1.66487744976166,10.3015948919053));
#13906=CARTESIAN_POINT('Ctrl Pts',(6.22237064400853,-1.64519198609486,10.303856032291));
#13907=CARTESIAN_POINT('Ctrl Pts',(6.25104729766808,-1.62476740026133,10.3061171726767));
#13908=CARTESIAN_POINT('Ctrl Pts',(6.30716481321017,-1.58479840574191,10.3105420118592));
#13909=CARTESIAN_POINT('Ctrl Pts',(6.36132690120277,-1.54183465873047,10.3149668510417));
#13910=CARTESIAN_POINT('Ctrl Pts',(6.41319290414351,-1.49609544604702,10.3193916902243));
#13911=CARTESIAN_POINT('Ctrl Pts',(6.46590360890188,-1.44961131388067,10.3238885933695));
#13912=CARTESIAN_POINT('Ctrl Pts',(6.51624229576162,-1.40026072416253,10.3283854965147));
#13913=CARTESIAN_POINT('Ctrl Pts',(6.56388183109682,-1.34831999655796,10.33288239966));
#13914=CARTESIAN_POINT('Ctrl Pts',(6.61063286537051,-1.297347989393,10.3372954333218));
#13915=CARTESIAN_POINT('Ctrl Pts',(6.65478420930858,-1.2438820088483,10.3417084669836));
#13916=CARTESIAN_POINT('Ctrl Pts',(6.69606156793214,-1.18822239078717,10.3461215006454));
#13917=CARTESIAN_POINT('Ctrl Pts',(6.73731423946764,-1.13259606152983,10.3505318949681));
#13918=CARTESIAN_POINT('Ctrl Pts',(6.77569603923256,-1.07477909471519,10.3549422892907));
#13919=CARTESIAN_POINT('Ctrl Pts',(6.8109729785983,-1.01510481456597,10.3593526836133));
#13920=CARTESIAN_POINT('Ctrl Pts',(6.84624120760493,-0.955445268813201,
10.3637619889492));
#13921=CARTESIAN_POINT('Ctrl Pts',(6.87840584553228,-0.893929747592757,
10.3681712942851));
#13922=CARTESIAN_POINT('Ctrl Pts',(6.90727729444706,-0.830918862394405,
10.372580599621));
#13923=CARTESIAN_POINT('Ctrl Pts',(6.93714461717892,-0.765734518879353,
10.3771419967951));
#13924=CARTESIAN_POINT('Ctrl Pts',(6.96348712604202,-0.698950254759972,
10.3817033939691));
#13925=CARTESIAN_POINT('Ctrl Pts',(6.98614865883704,-0.630988819497452,
10.3862647911432));
#13926=CARTESIAN_POINT('Ctrl Pts',(7.00808028594709,-0.565216355228417,
10.3906792702002));
#13927=CARTESIAN_POINT('Ctrl Pts',(7.02656439386085,-0.498341915087311,
10.3950937492571));
#13928=CARTESIAN_POINT('Ctrl Pts',(7.04151065576395,-0.430762748060807,
10.3995082283141));
#13929=CARTESIAN_POINT('Ctrl Pts',(7.05720305666604,-0.35980993133084,10.4041430845467));
#13930=CARTESIAN_POINT('Ctrl Pts',(7.06899502657416,-0.288080797450994,
10.4087779407793));
#13931=CARTESIAN_POINT('Ctrl Pts',(7.0768433357553,-0.216042567934474,10.4134127970119));
#13932=CARTESIAN_POINT('Ctrl Pts',(7.08469164493643,-0.144004338417935,
10.4180476532445));
#13933=CARTESIAN_POINT('Ctrl Pts',(7.08859633704874,-0.0716576417186778,
10.4226825094771));
#13934=CARTESIAN_POINT('Ctrl Pts',(7.08857708451418,0.000531987659116302,
10.4273173657097));
#13935=CARTESIAN_POINT('Origin',(5.09382715545311,0.,-6.77268258743872));
#13936=CARTESIAN_POINT('',(7.08573554628195,0.000892988623384845,11.3854254802821));
#13937=CARTESIAN_POINT('',(7.08797502715347,-0.00179838111111824,11.2273170635307));
#13938=CARTESIAN_POINT('',(7.08857715545311,8.3550772080578E-14,-6.77268258743872));
#13939=CARTESIAN_POINT('Ctrl Pts',(7.08857700164749,0.000783331027041838,
11.3870615703915));
#13940=CARTESIAN_POINT('Ctrl Pts',(7.08859050212995,-0.0335956025044396,
11.3849657369292));
#13941=CARTESIAN_POINT('Ctrl Pts',(7.08771523812136,-0.067967775722241,
11.3828458996653));
#13942=CARTESIAN_POINT('Ctrl Pts',(7.0854599564119,-0.111886118516987,11.3800989790134));
#13943=CARTESIAN_POINT('Ctrl Pts',(7.08489844898603,-0.121469404999907,
11.3794972526833));
#13944=CARTESIAN_POINT('Ctrl Pts',(7.08376269282117,-0.138719976608432,
11.3784097358079));
#13945=CARTESIAN_POINT('Ctrl Pts',(7.08321324344236,-0.146388746298036,
11.3779247219182));
#13946=CARTESIAN_POINT('Ctrl Pts',(7.08200019851094,-0.162048797123054,
11.3769310261121));
#13947=CARTESIAN_POINT('Ctrl Pts',(7.08133272365181,-0.170039628061656,
11.3764222321024));
#13948=CARTESIAN_POINT('Ctrl Pts',(7.07978810543651,-0.187277727010127,
11.3753207857812));
#13949=CARTESIAN_POINT('Ctrl Pts',(7.07889451733559,-0.196523296030458,
11.3747276303283));
#13950=CARTESIAN_POINT('Ctrl Pts',(7.07629189812463,-0.221619654077708,
11.3731108712311));
#13951=CARTESIAN_POINT('Ctrl Pts',(7.07445739048664,-0.237456469029167,
11.3720833697502));
#13952=CARTESIAN_POINT('Ctrl Pts',(7.06493459325003,-0.311851079412598,
11.3672213034655));
#13953=CARTESIAN_POINT('Ctrl Pts',(7.05483863455043,-0.370065422645639,
11.3633122878388));
#13954=CARTESIAN_POINT('Ctrl Pts',(7.00214150058168,-0.610099164649372,
11.346751212321));
#13955=CARTESIAN_POINT('Ctrl Pts',(6.93671349231064,-0.785899920915602,
11.3334378185118));
#13956=CARTESIAN_POINT('Ctrl Pts',(6.82806189668402,-0.986497642712622,
11.3179319640882));
#13957=CARTESIAN_POINT('Ctrl Pts',(6.80717455467169,-1.0223448489466,11.3151529315244));
#13958=CARTESIAN_POINT('Ctrl Pts',(6.78037417045649,-1.06520843276605,11.3118429187444));
#13959=CARTESIAN_POINT('Ctrl Pts',(6.77551285210947,-1.07286675044914,11.3112520534972));
#13960=CARTESIAN_POINT('Ctrl Pts',(6.76780391671225,-1.0848299401623,11.3103302080942));
#13961=CARTESIAN_POINT('Ctrl Pts',(6.76499161690613,-1.08915726162217,11.3099969979051));
#13962=CARTESIAN_POINT('Ctrl Pts',(6.75968340657217,-1.09725610768888,11.3093738980191));
#13963=CARTESIAN_POINT('Ctrl Pts',(6.75719148820311,-1.10103002331704,11.3090837685017));
#13964=CARTESIAN_POINT('Ctrl Pts',(6.75145030982186,-1.1096608427009,11.3084207193772));
#13965=CARTESIAN_POINT('Ctrl Pts',(6.74819252600374,-1.11451196966086,11.3080483734133));
#13966=CARTESIAN_POINT('Ctrl Pts',(6.7394326235441,-1.12743319212184,11.3070573058941));
#13967=CARTESIAN_POINT('Ctrl Pts',(6.73389239170094,-1.13547742786139,11.3064410356748));
#13968=CARTESIAN_POINT('Ctrl Pts',(6.68833390002943,-1.20059772016784,11.3014552649411));
#13969=CARTESIAN_POINT('Ctrl Pts',(6.64540341735061,-1.25558749182682,11.2972640011223));
#13970=CARTESIAN_POINT('Ctrl Pts',(6.50112251675087,-1.42166434451098,11.2842763383867));
#13971=CARTESIAN_POINT('Ctrl Pts',(6.39006625285841,-1.5236062553347,11.2757615618428));
#13972=CARTESIAN_POINT('Ctrl Pts',(6.23375663532229,-1.63751289683915,11.2642325375425));
#13973=CARTESIAN_POINT('Ctrl Pts',(6.19808769398939,-1.66177495709315,11.261631546079));
#13974=CARTESIAN_POINT('Ctrl Pts',(6.14458229319352,-1.69568573173536,11.2577518704288));
#13975=CARTESIAN_POINT('Ctrl Pts',(6.12733935837669,-1.70624996479905,11.2565048652517));
#13976=CARTESIAN_POINT('Ctrl Pts',(6.09969239175197,-1.72261559235524,11.254508801344));
#13977=CARTESIAN_POINT('Ctrl Pts',(6.08939159825758,-1.72858924654958,11.2537658320926));
#13978=CARTESIAN_POINT('Ctrl Pts',(6.0697367374453,-1.73975356863666,11.2523491851439));
#13979=CARTESIAN_POINT('Ctrl Pts',(6.06039316513557,-1.74496192898744,11.2516761624429));
#13980=CARTESIAN_POINT('Ctrl Pts',(6.04398366350237,-1.75393679448646,11.2504947016232));
#13981=CARTESIAN_POINT('Ctrl Pts',(6.03693604773138,-1.75773640888276,11.2499874510321));
#13982=CARTESIAN_POINT('Ctrl Pts',(6.02315108676149,-1.7650615889023,11.248995518425));
#13983=CARTESIAN_POINT('Ctrl Pts',(6.01641607331925,-1.76859126649599,11.2485109923619));
#13984=CARTESIAN_POINT('Ctrl Pts',(6.00037496040749,-1.77688151121632,11.2473571495161));
#13985=CARTESIAN_POINT('Ctrl Pts',(5.99105137126729,-1.78160756825438,11.2466866400883));
#13986=CARTESIAN_POINT('Ctrl Pts',(5.96281189524195,-1.79564405509356,11.2446559779213));
#13987=CARTESIAN_POINT('Ctrl Pts',(5.94378561982559,-1.80472784738692,11.2432880633953));
#13988=CARTESIAN_POINT('Ctrl Pts',(5.77400919200274,-1.88250470529182,11.2310801496649));
#13989=CARTESIAN_POINT('Ctrl Pts',(5.6154170001361,-1.93245812405543,11.2195839429194));
#13990=CARTESIAN_POINT('Ctrl Pts',(5.37918533188267,-1.97564056366196,11.2028492990731));
#13991=CARTESIAN_POINT('Ctrl Pts',(5.30515417568186,-1.98492498818679,11.1976716347176));
#13992=CARTESIAN_POINT('Ctrl Pts',(5.20693799968771,-1.9916837846586,11.1910106874793));
#13993=CARTESIAN_POINT('Ctrl Pts',(5.18307430131863,-1.99289573582765,11.1894086136156));
#13994=CARTESIAN_POINT('Ctrl Pts',(5.14285593274497,-1.99421436796962,11.1867421270537));
#13995=CARTESIAN_POINT('Ctrl Pts',(5.1265117323196,-1.99454920372412,11.1856678247984));
#13996=CARTESIAN_POINT('Ctrl Pts',(5.10363021598478,-1.99473661523291,11.1841785561112));
#13997=CARTESIAN_POINT('Ctrl Pts',(5.09709545075546,-1.99475802675018,11.1837549153987));
#13998=CARTESIAN_POINT('Ctrl Pts',(5.08594642630417,-1.99473976928282,11.1830351410441));
#13999=CARTESIAN_POINT('Ctrl Pts',(5.08133222486416,-1.99471620323393,11.1827381295447));
#14000=CARTESIAN_POINT('Ctrl Pts',(5.07242381926647,-1.99463979239863,11.1821664483625));
#14001=CARTESIAN_POINT('Ctrl Pts',(5.06812967580166,-1.99458909166899,11.1818916559751));
#14002=CARTESIAN_POINT('Ctrl Pts',(5.05654490179536,-1.99441489252716,11.1811523340471));
#14003=CARTESIAN_POINT('Ctrl Pts',(5.04925464417529,-1.99426528454597,11.1806892347172));
#14004=CARTESIAN_POINT('Ctrl Pts',(5.02203622625401,-1.99355738795772,11.1789677348685));
#14005=CARTESIAN_POINT('Ctrl Pts',(5.00211521229091,-1.99274032101949,11.1777227857297));
#14006=CARTESIAN_POINT('Ctrl Pts',(4.8428969442853,-1.98381712282033,11.1678688644336));
#14007=CARTESIAN_POINT('Ctrl Pts',(4.70476982860234,-1.96141304161784,11.1598908889779));
#14008=CARTESIAN_POINT('Ctrl Pts',(4.48668418079415,-1.90207204543683,11.1467494400709));
#14009=CARTESIAN_POINT('Ctrl Pts',(4.40483854025718,-1.87397803108736,11.1416888867652));
#14010=CARTESIAN_POINT('Ctrl Pts',(4.28033488005824,-1.82197942609904,11.1335531348843));
#14011=CARTESIAN_POINT('Ctrl Pts',(4.23629105254116,-1.80166866114592,11.1305856577438));
#14012=CARTESIAN_POINT('Ctrl Pts',(4.1804828045708,-1.77342254597474,11.1266864497802));
#14013=CARTESIAN_POINT('Ctrl Pts',(4.16800003325703,-1.76693790317709,11.1258051089959));
#14014=CARTESIAN_POINT('Ctrl Pts',(4.14783432556259,-1.75618971339038,11.1243658083576));
#14015=CARTESIAN_POINT('Ctrl Pts',(4.14010900043112,-1.75200639850894,11.1238106794371));
#14016=CARTESIAN_POINT('Ctrl Pts',(4.12530447387874,-1.7438627165738,11.1227395026326));
#14017=CARTESIAN_POINT('Ctrl Pts',(4.11822128787983,-1.73990992495575,11.1222237319706));
#14018=CARTESIAN_POINT('Ctrl Pts',(4.10203592977094,-1.73074773220773,11.1210375544509));
#14019=CARTESIAN_POINT('Ctrl Pts',(4.09295039931226,-1.72550956530975,11.1203661264057));
#14020=CARTESIAN_POINT('Ctrl Pts',(4.06417187168313,-1.70861384312165,11.1182212904702));
#14021=CARTESIAN_POINT('Ctrl Pts',(4.04463856380536,-1.69668927486082,11.1167382876586));
#14022=CARTESIAN_POINT('Ctrl Pts',(3.88138193346995,-1.59312815524446,11.1041065818927));
#14023=CARTESIAN_POINT('Ctrl Pts',(3.74977047466984,-1.48376862296477,11.0922596469863));
#14024=CARTESIAN_POINT('Ctrl Pts',(3.56491759556801,-1.28516583036661,11.0733597123531));
#14025=CARTESIAN_POINT('Ctrl Pts',(3.50184737784965,-1.20615948013205,11.0663698761083));
#14026=CARTESIAN_POINT('Ctrl Pts',(3.43830522429634,-1.11284195408442,11.0589385943018));
#14027=CARTESIAN_POINT('Ctrl Pts',(3.43167463031966,-1.10291390378076,11.0581578424654));
#14028=CARTESIAN_POINT('Ctrl Pts',(3.42197913589062,-1.08811070413213,11.0570089357811));
#14029=CARTESIAN_POINT('Ctrl Pts',(3.41884571003396,-1.08328106438982,11.0566364730371));
#14030=CARTESIAN_POINT('Ctrl Pts',(3.41329793205102,-1.07464849208454,11.0559750457173));
#14031=CARTESIAN_POINT('Ctrl Pts',(3.41087551244865,-1.07085088640116,11.05568555786));
#14032=CARTESIAN_POINT('Ctrl Pts',(3.40563919110418,-1.06258029498531,11.0550583300518));
#14033=CARTESIAN_POINT('Ctrl Pts',(3.40283019423773,-1.05810432613117,11.054720910004));
#14034=CARTESIAN_POINT('Ctrl Pts',(3.39508664303426,-1.04565584326884,11.0537879472045));
#14035=CARTESIAN_POINT('Ctrl Pts',(3.39019038589964,-1.03765949938148,11.0531948382425));
#14036=CARTESIAN_POINT('Ctrl Pts',(3.36406701926906,-0.994312652124109,
11.0500112566252));
#14037=CARTESIAN_POINT('Ctrl Pts',(3.34388188387452,-0.958342249428195,
11.0474819839229));
#14038=CARTESIAN_POINT('Ctrl Pts',(3.31179863076767,-0.896770059389174,
11.0432946766284));
#14039=CARTESIAN_POINT('Ctrl Pts',(3.29930331114055,-0.871496693820793,
11.0416147334492));
#14040=CARTESIAN_POINT('Ctrl Pts',(3.24229803838006,-0.749767388698813,
11.0336679963512));
#14041=CARTESIAN_POINT('Ctrl Pts',(3.20500345326026,-0.650121359538879,
11.027580877731));
#14042=CARTESIAN_POINT('Ctrl Pts',(3.14876826736442,-0.453289119408947,
11.0156221138267));
#14043=CARTESIAN_POINT('Ctrl Pts',(3.12876766603665,-0.356739327193686,
11.0097835050644));
#14044=CARTESIAN_POINT('Ctrl Pts',(3.11291087850071,-0.235702744641075,
11.0022611009819));
#14045=CARTESIAN_POINT('Ctrl Pts',(3.11025977963813,-0.212239187226894,
11.0007940487766));
#14046=CARTESIAN_POINT('Ctrl Pts',(3.1070102052518,-0.178048314735636,10.9986411443714));
#14047=CARTESIAN_POINT('Ctrl Pts',(3.10608083106555,-0.167353932346221,
10.9979656079912));
#14048=CARTESIAN_POINT('Ctrl Pts',(3.10460005185348,-0.148556547509568,
10.9967742492367));
#14049=CARTESIAN_POINT('Ctrl Pts',(3.10401172521529,-0.140456640715687,
10.9962595908666));
#14050=CARTESIAN_POINT('Ctrl Pts',(3.10296280396824,-0.124682781596197,
10.9952547276015));
#14051=CARTESIAN_POINT('Ctrl Pts',(3.10249707686687,-0.117009304941435,
10.9947646923633));
#14052=CARTESIAN_POINT('Ctrl Pts',(3.10136640753617,-0.0964116472297227,
10.993445989413));
#14053=CARTESIAN_POINT('Ctrl Pts',(3.10078287021135,-0.0834835417316138,
10.9926148017454));
#14054=CARTESIAN_POINT('Ctrl Pts',(3.09908385627865,-0.0354758387549812,
10.9895147212196));
#14055=CARTESIAN_POINT('Ctrl Pts',(3.09876851823717,-0.000376080368230205,
10.9872212428741));
#14056=CARTESIAN_POINT('Ctrl Pts',(3.1028860610232,0.236205784078398,10.9715719864317));
#14057=CARTESIAN_POINT('Ctrl Pts',(3.13691051066298,0.435988478456032,10.957256317076));
#14058=CARTESIAN_POINT('Ctrl Pts',(3.21774239621701,0.680020182160489,10.9396203170828));
#14059=CARTESIAN_POINT('Ctrl Pts',(3.23743488298876,0.732072693490488,10.9358610974789));
#14060=CARTESIAN_POINT('Ctrl Pts',(3.26313156028253,0.792260968475792,10.9315697331184));
#14061=CARTESIAN_POINT('Ctrl Pts',(3.26705017335975,0.801255060180023,10.9309299703773));
#14062=CARTESIAN_POINT('Ctrl Pts',(3.27319649702166,0.815082747470845,10.9299491253994));
#14063=CARTESIAN_POINT('Ctrl Pts',(3.27537739754418,0.819936801955177,10.9296053348741));
#14064=CARTESIAN_POINT('Ctrl Pts',(3.27943880886156,0.828880419470953,10.9289729469639));
#14065=CARTESIAN_POINT('Ctrl Pts',(3.28131372840238,0.832972328161857,10.9286840304972));
#14066=CARTESIAN_POINT('Ctrl Pts',(3.28559775454483,0.842239025692224,10.9280306546167));
#14067=CARTESIAN_POINT('Ctrl Pts',(3.28801522939811,0.847409837306923,10.9276667119581));
#14068=CARTESIAN_POINT('Ctrl Pts',(3.2943453019036,0.86079932251171,10.9267257898313));
#14069=CARTESIAN_POINT('Ctrl Pts',(3.29829206810475,0.86900182529183,10.9261508309693));
#14070=CARTESIAN_POINT('Ctrl Pts',(3.32490261567474,0.923350767754326,10.9223490455802));
#14071=CARTESIAN_POINT('Ctrl Pts',(3.34928908238131,0.9686374783957,10.9192187352752));
#14072=CARTESIAN_POINT('Ctrl Pts',(3.40398899219318,1.0614349121035,10.9127791978383));
#14073=CARTESIAN_POINT('Ctrl Pts',(3.43461928442492,1.10870507240111,10.9094839109244));
#14074=CARTESIAN_POINT('Ctrl Pts',(3.526683245807,1.23840411003592,10.9002256783233));
#14075=CARTESIAN_POINT('Ctrl Pts',(3.59253938965534,1.31746690734485,10.894311569077));
#14076=CARTESIAN_POINT('Ctrl Pts',(3.71640414327561,1.44476254392003,10.8837833589001));
#14077=CARTESIAN_POINT('Ctrl Pts',(3.77159080436036,1.49543375269944,10.8792626418684));
#14078=CARTESIAN_POINT('Ctrl Pts',(3.84190273511683,1.55305194431792,10.8736113018938));
#14079=CARTESIAN_POINT('Ctrl Pts',(3.85443727387511,1.56307318890195,10.8726078900301));
#14080=CARTESIAN_POINT('Ctrl Pts',(3.87436093855319,1.57861163853467,10.8710185557582));
#14081=CARTESIAN_POINT('Ctrl Pts',(3.88166991595748,1.58423084858865,10.8704366724332));
#14082=CARTESIAN_POINT('Ctrl Pts',(3.89541520311462,1.5946475450852,10.8693444031634));
#14083=CARTESIAN_POINT('Ctrl Pts',(3.90184205029887,1.59945725374903,10.8688345092295));
#14084=CARTESIAN_POINT('Ctrl Pts',(3.91626784426315,1.61011796043722,10.8676917104519));
#14085=CARTESIAN_POINT('Ctrl Pts',(3.92428167302932,1.61594837064765,10.8670580272072));
#14086=CARTESIAN_POINT('Ctrl Pts',(3.94469914662214,1.63057153769293,10.865446299987));
#14087=CARTESIAN_POINT('Ctrl Pts',(3.9571603116017,1.6392825214536,10.864465177593));
#14088=CARTESIAN_POINT('Ctrl Pts',(4.03379632819752,1.69156102246822,10.8584454991326));
#14089=CARTESIAN_POINT('Ctrl Pts',(4.10036009073022,1.73149201988066,10.8532732244031));
#14090=CARTESIAN_POINT('Ctrl Pts',(4.28027821191365,1.82562808503646,10.8394432889076));
#14091=CARTESIAN_POINT('Ctrl Pts',(4.39672232160349,1.87318451079591,10.8306231485748));
#14092=CARTESIAN_POINT('Ctrl Pts',(4.58678666636478,1.93061530956486,10.8168572315459));
#14093=CARTESIAN_POINT('Ctrl Pts',(4.65784073161889,1.94789207557644,10.8118482390382));
#14094=CARTESIAN_POINT('Ctrl Pts',(4.74459659578435,1.96399986611261,10.806010913221));
#14095=CARTESIAN_POINT('Ctrl Pts',(4.75953574276866,1.9665977581881,10.8050156409445));
#14096=CARTESIAN_POINT('Ctrl Pts',(4.78076281291103,1.97004022502322,10.8036168358518));
#14097=CARTESIAN_POINT('Ctrl Pts',(4.78702694579063,1.97102547035342,10.8032059399985));
#14098=CARTESIAN_POINT('Ctrl Pts',(4.79782329513392,1.97267084221676,10.8025011350625));
#14099=CARTESIAN_POINT('Ctrl Pts',(4.80235325152159,1.97334525669059,10.8022064367495));
#14100=CARTESIAN_POINT('Ctrl Pts',(4.81118770882578,1.97462943482469,10.8016337463239));
#14101=CARTESIAN_POINT('Ctrl Pts',(4.81549189529821,1.97524073102381,10.8013556639534));
#14102=CARTESIAN_POINT('Ctrl Pts',(4.82728710209811,1.97687660881291,10.8005960811779));
#14103=CARTESIAN_POINT('Ctrl Pts',(4.83478209645489,1.9778726926405,10.8001161533745));
#14104=CARTESIAN_POINT('Ctrl Pts',(4.86394534797918,1.98157986708738,10.7982587205718));
#14105=CARTESIAN_POINT('Ctrl Pts',(4.88565278766873,1.98397780721929,10.7968975487706));
#14106=CARTESIAN_POINT('Ctrl Pts',(5.10214214581195,2.00430002365368,10.7834962197265));
#14107=CARTESIAN_POINT('Ctrl Pts',(5.29854105444291,1.99384114128001,10.7726434854575));
#14108=CARTESIAN_POINT('Ctrl Pts',(5.56187053028585,1.94043716977198,10.7567002408052));
#14109=CARTESIAN_POINT('Ctrl Pts',(5.63258568713428,1.92200376887631,10.7522865357292));
#14110=CARTESIAN_POINT('Ctrl Pts',(5.71730841999873,1.89487540820673,10.7467553042911));
#14111=CARTESIAN_POINT('Ctrl Pts',(5.73243159710898,1.88983227929282,10.7457584269983));
#14112=CARTESIAN_POINT('Ctrl Pts',(5.75618080472414,1.88159500852578,10.7441771263741));
#14113=CARTESIAN_POINT('Ctrl Pts',(5.76484817845943,1.87852147044783,10.7435966730059));
#14114=CARTESIAN_POINT('Ctrl Pts',(5.78104285711955,1.87265229392335,10.7425056855572));
#14115=CARTESIAN_POINT('Ctrl Pts',(5.78857516059319,1.86987091555283,10.7419956327077));
#14116=CARTESIAN_POINT('Ctrl Pts',(5.80539565774374,1.8635441147646,10.7408506432768));
#14117=CARTESIAN_POINT('Ctrl Pts',(5.81467450011127,1.85997459685158,10.7402149145381));
#14118=CARTESIAN_POINT('Ctrl Pts',(5.8381706128949,1.85073354958053,10.7385944649756));
#14119=CARTESIAN_POINT('Ctrl Pts',(5.85234979485469,1.84496754391589,10.737606607556));
#14120=CARTESIAN_POINT('Ctrl Pts',(5.94016140901111,1.80807533354587,10.7314252850219));
#14121=CARTESIAN_POINT('Ctrl Pts',(6.01192456389537,1.77271327841365,10.7260894304148));
#14122=CARTESIAN_POINT('Ctrl Pts',(6.20215408152322,1.66432137021369,10.7111586952375));
#14123=CARTESIAN_POINT('Ctrl Pts',(6.3154133706686,1.58305916377974,10.7013471941833));
#14124=CARTESIAN_POINT('Ctrl Pts',(6.46761859198697,1.44772465904652,10.6873094853261));
#14125=CARTESIAN_POINT('Ctrl Pts',(6.51383332505937,1.40242428366876,10.6829165666868));
#14126=CARTESIAN_POINT('Ctrl Pts',(6.56466367532966,1.34750528935272,10.6780064589811));
#14127=CARTESIAN_POINT('Ctrl Pts',(6.57150099053989,1.3400039628807,10.6773442576048));
#14128=CARTESIAN_POINT('Ctrl Pts',(6.58188366204331,1.32843685791351,10.6763364580841));
#14129=CARTESIAN_POINT('Ctrl Pts',(6.58547015875157,1.32440847348426,10.6759879189442));
#14130=CARTESIAN_POINT('Ctrl Pts',(6.59201658600006,1.31699514439885,10.6753510496281));
#14131=CARTESIAN_POINT('Ctrl Pts',(6.59498140787082,1.31361474239271,10.675062365685));
#14132=CARTESIAN_POINT('Ctrl Pts',(6.6016260710158,1.30598681975566,10.6744147890303));
#14133=CARTESIAN_POINT('Ctrl Pts',(6.6052994028311,1.30173376325867,10.6740563730353));
#14134=CARTESIAN_POINT('Ctrl Pts',(6.61603914817315,1.28919232093253,10.6730070337502));
#14135=CARTESIAN_POINT('Ctrl Pts',(6.6230558424132,1.28086136121408,10.6723196145986));
#14136=CARTESIAN_POINT('Ctrl Pts',(6.6933905249563,1.19595071159921,10.6654052068969));
#14137=CARTESIAN_POINT('Ctrl Pts',(6.75097975288173,1.11478778209156,10.6595428744423));
#14138=CARTESIAN_POINT('Ctrl Pts',(6.86735588215672,0.921691312295174,10.6463971792345));
#14139=CARTESIAN_POINT('Ctrl Pts',(6.92204271454937,0.807802950007679,10.6391713742038));
#14140=CARTESIAN_POINT('Ctrl Pts',(6.98643114614844,0.633011710764672,10.6280315007438));
#14141=CARTESIAN_POINT('Ctrl Pts',(7.00467516930955,0.575597519728701,10.6243687102326));
#14142=CARTESIAN_POINT('Ctrl Pts',(7.024206003035,0.502884216341028,10.6196819660917));
#14143=CARTESIAN_POINT('Ctrl Pts',(7.02795296433797,0.488274887758236,10.6187380274384));
#14144=CARTESIAN_POINT('Ctrl Pts',(7.03367269191741,0.464874181844254,10.6172218024364));
#14145=CARTESIAN_POINT('Ctrl Pts',(7.03575223197809,0.456109310534919,10.6166529444937));
#14146=CARTESIAN_POINT('Ctrl Pts',(7.03957883339206,0.439480221324501,10.6155717607668));
#14147=CARTESIAN_POINT('Ctrl Pts',(7.04133776661476,0.431618898382836,10.6150598261905));
#14148=CARTESIAN_POINT('Ctrl Pts',(7.0452222297898,0.413750508949665,10.6138942895309));
#14149=CARTESIAN_POINT('Ctrl Pts',(7.04731847756764,0.403737374789287,10.6132397694319));
#14150=CARTESIAN_POINT('Ctrl Pts',(7.05254626365009,0.377771502294452,10.6115387322755));
#14151=CARTESIAN_POINT('Ctrl Pts',(7.05555991799737,0.36179606860488,10.6104885189985));
#14152=CARTESIAN_POINT('Ctrl Pts',(7.07847589052951,0.231601106159984,10.6018980869804));
#14153=CARTESIAN_POINT('Ctrl Pts',(7.08857715545954,0.115902333697236,10.5940476725223));
#14154=CARTESIAN_POINT('Ctrl Pts',(7.08857715545311,-1.10669147457276E-10,
10.5860251696756));
#14155=CARTESIAN_POINT('Ctrl Pts',(7.09165123813443,0.000533538373458679,
10.4273174125613));
#14156=CARTESIAN_POINT('Ctrl Pts',(7.09175584924485,0.0297929794135023,
10.4291930904358));
#14157=CARTESIAN_POINT('Ctrl Pts',(7.07793077862856,0.718427657987238,10.4733445261464));
#14158=CARTESIAN_POINT('Ctrl Pts',(6.28614855086912,2.03262338503281,10.5597717196931));
#14159=CARTESIAN_POINT('Ctrl Pts',(4.03585361648675,2.10567798773344,10.6865989932013));
#14160=CARTESIAN_POINT('Ctrl Pts',(2.75131770239386,0.256588624035499,10.8134262667095));
#14161=CARTESIAN_POINT('Ctrl Pts',(3.60511495718796,-1.82672508052752,10.9402535402178));
#14162=CARTESIAN_POINT('Ctrl Pts',(5.81786594038741,-2.24253297202115,11.067080813726));
#14163=CARTESIAN_POINT('Ctrl Pts',(6.98867395944926,-1.01178906555039,11.1627686548303));
#14164=CARTESIAN_POINT('Ctrl Pts',(7.08951450949766,-0.176350808701007,
11.2161807380985));
#14165=CARTESIAN_POINT('Ctrl Pts',(7.08797502715347,-0.00179838111111824,
11.2273170635307));
#14166=CARTESIAN_POINT('Origin',(5.09382715545311,0.,-6.77268258743872));
#14167=CARTESIAN_POINT('',(7.08857671409759,0.0013269467482341,12.1854076497708));
#14168=CARTESIAN_POINT('',(7.08857715545311,1.48164940157807E-8,12.0255409243712));
#14169=CARTESIAN_POINT('',(7.08857715545311,8.3550772080578E-14,-6.77268258743872));
#14170=CARTESIAN_POINT('Ctrl Pts',(7.08570589435167,0.000894132952252917,
11.3854084069082));
#14171=CARTESIAN_POINT('Ctrl Pts',(7.08680590574586,0.276931583514048,11.4029688699668));
#14172=CARTESIAN_POINT('Ctrl Pts',(6.90460270567564,1.21611910765721,11.4628050908614));
#14173=CARTESIAN_POINT('Ctrl Pts',(5.4714363682364,2.32605240372542,11.5649170695921));
#14174=CARTESIAN_POINT('Ctrl Pts',(3.34667780576886,1.5813865206481,11.6917443431003));
#14175=CARTESIAN_POINT('Ctrl Pts',(2.81680521163759,-0.606947692680927,
11.8185716166085));
#14176=CARTESIAN_POINT('Ctrl Pts',(4.3654468926145,-2.24101245944887,11.9453988901168));
#14177=CARTESIAN_POINT('Ctrl Pts',(6.49966051365026,-1.84456996298104,12.0676771988713));
#14178=CARTESIAN_POINT('Ctrl Pts',(7.08670906604921,-0.587748414857904,
12.1476797497898));
#14179=CARTESIAN_POINT('Ctrl Pts',(7.09088662258869,0.00131120050381758,
12.1854065428722));
#14180=CARTESIAN_POINT('Ctrl Pts',(7.08857715545311,1.48164940157807E-8,
12.0255409243712));
#14181=CARTESIAN_POINT('Ctrl Pts',(7.08857715560486,-0.0204294858188712,
12.0241991575096));
#14182=CARTESIAN_POINT('Ctrl Pts',(7.08826330894787,-0.0408607784063718,
12.0228667225922));
#14183=CARTESIAN_POINT('Ctrl Pts',(7.08717163368709,-0.076375701020997,
12.0205665158892));
#14184=CARTESIAN_POINT('Ctrl Pts',(7.08653653486394,-0.0914593163802701,
12.0195945812698));
#14185=CARTESIAN_POINT('Ctrl Pts',(7.08524929289252,-0.115527185493051,
12.0180513772495));
#14186=CARTESIAN_POINT('Ctrl Pts',(7.0847074389005,-0.124516510658469,12.017476695354));
#14187=CARTESIAN_POINT('Ctrl Pts',(7.08356622597029,-0.141529969751081,
12.0163921571722));
#14188=CARTESIAN_POINT('Ctrl Pts',(7.08297915809114,-0.149554720992709,
12.0158819286443));
#14189=CARTESIAN_POINT('Ctrl Pts',(7.0815371704763,-0.167751779511177,12.014727810809));
#14190=CARTESIAN_POINT('Ctrl Pts',(7.08065268490258,-0.177921570061504,
12.0140848569458));
#14191=CARTESIAN_POINT('Ctrl Pts',(7.07816258338,-0.204212978209397,12.0124276916232));
#14192=CARTESIAN_POINT('Ctrl Pts',(7.07643854125095,-0.220322826678904,
12.0114171805031));
#14193=CARTESIAN_POINT('Ctrl Pts',(7.06146836141441,-0.345745910053498,
12.0035842620008));
#14194=CARTESIAN_POINT('Ctrl Pts',(7.03938725592229,-0.45382016427159,11.9970536774645));
#14195=CARTESIAN_POINT('Ctrl Pts',(7.00416595533655,-0.574344306882903,
11.9897252512486));
#14196=CARTESIAN_POINT('Ctrl Pts',(6.99966543581773,-0.589106245051875,
11.9888265709252));
#14197=CARTESIAN_POINT('Ctrl Pts',(6.96112767873423,-0.710445995464346,
11.9814224742288));
#14198=CARTESIAN_POINT('Ctrl Pts',(6.9183529365093,-0.814031239082437,11.975002622826));
#14199=CARTESIAN_POINT('Ctrl Pts',(6.84639343525565,-0.953723564535285,
11.9655610833747));
#14200=CARTESIAN_POINT('Ctrl Pts',(6.82429869269057,-0.993249597015682,
11.9627929142148));
#14201=CARTESIAN_POINT('Ctrl Pts',(6.79633730320581,-1.03950174723979,11.9593950391903));
#14202=CARTESIAN_POINT('Ctrl Pts',(6.79174445096947,-1.04698688466185,11.958840043649));
#14203=CARTESIAN_POINT('Ctrl Pts',(6.78413825013445,-1.05920130749264,11.95792557125));
#14204=CARTESIAN_POINT('Ctrl Pts',(6.78115406260131,-1.06394873615532,11.9575679363026));
#14205=CARTESIAN_POINT('Ctrl Pts',(6.77574238880087,-1.07247792737476,11.9569213133934));
#14206=CARTESIAN_POINT('Ctrl Pts',(6.77332209942813,-1.07626413540411,11.956632797633));
#14207=CARTESIAN_POINT('Ctrl Pts',(6.76796557779976,-1.08458160514534,11.9559957279569));
#14208=CARTESIAN_POINT('Ctrl Pts',(6.76502376783589,-1.08910908383634,11.95564681605));
#14209=CARTESIAN_POINT('Ctrl Pts',(6.7564853416555,-1.10213376847607,11.954637022104));
#14210=CARTESIAN_POINT('Ctrl Pts',(6.7508421440695,-1.11060002016434,11.9539731822478));
#14211=CARTESIAN_POINT('Ctrl Pts',(6.70844060907201,-1.17317067295451,11.9490135126114));
#14212=CARTESIAN_POINT('Ctrl Pts',(6.66910923265989,-1.22547564890171,11.9445694547647));
#14213=CARTESIAN_POINT('Ctrl Pts',(6.53604804838631,-1.38541604178657,11.9302250166383));
#14214=CARTESIAN_POINT('Ctrl Pts',(6.4332983087131,-1.48499215679976,11.9201537398576));
#14215=CARTESIAN_POINT('Ctrl Pts',(6.26097273160203,-1.61943116664853,11.905281212892));
#14216=CARTESIAN_POINT('Ctrl Pts',(6.19852110929785,-1.66266046802766,11.9002234551428));
#14217=CARTESIAN_POINT('Ctrl Pts',(6.12083401567374,-1.71012092248311,11.8943167379608));
#14218=CARTESIAN_POINT('Ctrl Pts',(6.10782797010078,-1.71786467139318,11.8933400229155));
#14219=CARTESIAN_POINT('Ctrl Pts',(6.08617834223766,-1.73042322337279,11.8917338566114));
#14220=CARTESIAN_POINT('Ctrl Pts',(6.07758501817901,-1.73532299103841,11.8911013670765));
#14221=CARTESIAN_POINT('Ctrl Pts',(6.06195102701605,-1.7440837709808,11.8899596352602));
#14222=CARTESIAN_POINT('Ctrl Pts',(6.05492286426732,-1.74796655358801,11.8894496241813));
#14223=CARTESIAN_POINT('Ctrl Pts',(6.03975647963111,-1.75622625499351,11.8883559158525));
#14224=CARTESIAN_POINT('Ctrl Pts',(6.03161087738241,-1.7605892878742,11.8877727187404));
#14225=CARTESIAN_POINT('Ctrl Pts',(6.00916134239369,-1.77241393445275,11.8861767316648));
#14226=CARTESIAN_POINT('Ctrl Pts',(5.99479654652679,-1.7797589750001,11.8851680337521));
#14227=CARTESIAN_POINT('Ctrl Pts',(5.91197720593532,-1.82084663236703,11.8794210778035));
#14228=CARTESIAN_POINT('Ctrl Pts',(5.84171581341721,-1.85081509069313,11.874815299007));
#14229=CARTESIAN_POINT('Ctrl Pts',(5.66045126731508,-1.91611561703539,11.8634032207174));
#14230=CARTESIAN_POINT('Ctrl Pts',(5.5477619045618,-1.94589449072751,11.8567394609109));
#14231=CARTESIAN_POINT('Ctrl Pts',(5.34366366450904,-1.98112340814124,11.8446292804051));
#14232=CARTESIAN_POINT('Ctrl Pts',(5.25326984666581,-1.99043762429821,11.8392457949777));
#14233=CARTESIAN_POINT('Ctrl Pts',(5.15162914606547,-1.99394240756791,11.8328685748772));
#14234=CARTESIAN_POINT('Ctrl Pts',(5.14068622328987,-1.9942295780237,11.8321777614457));
#14235=CARTESIAN_POINT('Ctrl Pts',(5.1241088498934,-1.99452809499195,11.8311241086831));
#14236=CARTESIAN_POINT('Ctrl Pts',(5.11847559462421,-1.99460566411278,11.8307648115901));
#14237=CARTESIAN_POINT('Ctrl Pts',(5.10834325609253,-1.99470225532085,11.8301161890694));
#14238=CARTESIAN_POINT('Ctrl Pts',(5.10384435611217,-1.99472992143752,11.829827345741));
#14239=CARTESIAN_POINT('Ctrl Pts',(5.09395892011331,-1.99475726816465,11.82919078955));
#14240=CARTESIAN_POINT('Ctrl Pts',(5.08857253677882,-1.99475035119417,11.8288427275511));
#14241=CARTESIAN_POINT('Ctrl Pts',(5.07307350750902,-1.99466767171319,11.8278378292703));
#14242=CARTESIAN_POINT('Ctrl Pts',(5.06296149916303,-1.9945368222858,11.8271780785227));
#14243=CARTESIAN_POINT('Ctrl Pts',(4.9893244100172,-1.99302385658667,11.8223457257424));
#14244=CARTESIAN_POINT('Ctrl Pts',(4.92590270814704,-1.98868413302647,11.8180331513315));
#14245=CARTESIAN_POINT('Ctrl Pts',(4.73095675971474,-1.9659533434419,11.8045132303469));
#14246=CARTESIAN_POINT('Ctrl Pts',(4.60097098022095,-1.93745808772483,11.795148782149));
#14247=CARTESIAN_POINT('Ctrl Pts',(4.39227811762146,-1.86932797264268,11.7801258880887));
#14248=CARTESIAN_POINT('Ctrl Pts',(4.31162072448025,-1.8370396955942,11.7743157675162));
#14249=CARTESIAN_POINT('Ctrl Pts',(4.21923743572319,-1.79286469300563,11.7676673568594));
#14250=CARTESIAN_POINT('Ctrl Pts',(4.20524096419635,-1.78596908955846,11.7666600742175));
#14251=CARTESIAN_POINT('Ctrl Pts',(4.18238002017592,-1.77437096537491,11.7650144701619));
#14252=CARTESIAN_POINT('Ctrl Pts',(4.17346777565167,-1.76976462311721,11.7643728422437));
#14253=CARTESIAN_POINT('Ctrl Pts',(4.15747921910262,-1.76134740781965,11.7632214583307));
#14254=CARTESIAN_POINT('Ctrl Pts',(4.15039051967552,-1.75756065792886,11.7627108707643));
#14255=CARTESIAN_POINT('Ctrl Pts',(4.13529524742915,-1.74937919189992,11.7616232558951));
#14256=CARTESIAN_POINT('Ctrl Pts',(4.12729555935203,-1.74497210692932,11.7610466800849));
#14257=CARTESIAN_POINT('Ctrl Pts',(4.10566921693358,-1.73286365205934,11.7594872295732));
#14258=CARTESIAN_POINT('Ctrl Pts',(4.09210229885574,-1.72505648651231,11.7585081390555));
#14259=CARTESIAN_POINT('Ctrl Pts',(4.01981514766311,-1.68231800636631,11.7532847599309));
#14260=CARTESIAN_POINT('Ctrl Pts',(3.96282341474003,-1.64454482738862,11.7491452045988));
#14261=CARTESIAN_POINT('Ctrl Pts',(3.77184146997626,-1.50333127156703,11.7350129599237));
#14262=CARTESIAN_POINT('Ctrl Pts',(3.64916789920824,-1.38585822686345,11.7255116645967));
#14263=CARTESIAN_POINT('Ctrl Pts',(3.51198603411108,-1.21622654812987,11.7124442578769));
#14264=CARTESIAN_POINT('Ctrl Pts',(3.48259247892641,-1.17700904896186,11.709456273408));
#14265=CARTESIAN_POINT('Ctrl Pts',(3.44955478681268,-1.12937003125684,11.7058130992666));
#14266=CARTESIAN_POINT('Ctrl Pts',(3.44448463001982,-1.12195254644654,11.7052454708539));
#14267=CARTESIAN_POINT('Ctrl Pts',(3.43629575591612,-1.10979700621703,11.7043141980256));
#14268=CARTESIAN_POINT('Ctrl Pts',(3.43314677012879,-1.10507935975399,11.7039525066836));
#14269=CARTESIAN_POINT('Ctrl Pts',(3.42753652478423,-1.09659624890082,11.7033015409498));
#14270=CARTESIAN_POINT('Ctrl Pts',(3.42506783427205,-1.09283581849832,11.7030127672697));
#14271=CARTESIAN_POINT('Ctrl Pts',(3.41969161091006,-1.08458579657519,11.7023787411732));
#14272=CARTESIAN_POINT('Ctrl Pts',(3.41678944820669,-1.08009291197126,11.7020331562719));
#14273=CARTESIAN_POINT('Ctrl Pts',(3.40854556981275,-1.06721710422248,11.7010420389919));
#14274=CARTESIAN_POINT('Ctrl Pts',(3.4032484887669,-1.05880599374926,11.7003937100007));
#14275=CARTESIAN_POINT('Ctrl Pts',(3.36702756727262,-1.00032686767989,11.6958819526625));
#14276=CARTESIAN_POINT('Ctrl Pts',(3.33827261477922,-0.948956004926795,
11.6918982132154));
#14277=CARTESIAN_POINT('Ctrl Pts',(3.26994381664234,-0.81312137884562,11.6814484010711));
#14278=CARTESIAN_POINT('Ctrl Pts',(3.23394406004819,-0.727015299442956,
11.6749088485831));
#14279=CARTESIAN_POINT('Ctrl Pts',(3.16241652549728,-0.515388887929364,
11.659390173647));
#14280=CARTESIAN_POINT('Ctrl Pts',(3.13290038855704,-0.38826583577615,11.6505252877003));
#14281=CARTESIAN_POINT('Ctrl Pts',(3.11387783629447,-0.243086001126109,
11.6410111930238));
#14282=CARTESIAN_POINT('Ctrl Pts',(3.11196853217163,-0.226994566722795,
11.6399644523661));
#14283=CARTESIAN_POINT('Ctrl Pts',(3.10917573533098,-0.200725219938103,
11.6382679406204));
#14284=CARTESIAN_POINT('Ctrl Pts',(3.10817400701529,-0.190560892639338,
11.6376145046309));
#14285=CARTESIAN_POINT('Ctrl Pts',(3.1065221425037,-0.172369358011783,11.6364502311264));
#14286=CARTESIAN_POINT('Ctrl Pts',(3.10584247403451,-0.164345123525658,
11.6359384823668));
#14287=CARTESIAN_POINT('Ctrl Pts',(3.10450489849324,-0.147328896534347,
11.6348570056964));
#14288=CARTESIAN_POINT('Ctrl Pts',(3.10385932275352,-0.138336094042632,
11.6342876733457));
#14289=CARTESIAN_POINT('Ctrl Pts',(3.10229433713584,-0.114250679488671,
11.6327685604097));
#14290=CARTESIAN_POINT('Ctrl Pts',(3.10148551122797,-0.099151281702897,
11.6318222328006));
#14291=CARTESIAN_POINT('Ctrl Pts',(3.09828939981654,-0.0233600746593698,
11.6271004173928));
#14292=CARTESIAN_POINT('Ctrl Pts',(3.09850312078127,0.0374126224863856,
11.6234064619461));
#14293=CARTESIAN_POINT('Ctrl Pts',(3.10779791010855,0.226210296203055,11.6121060131336));
#14294=CARTESIAN_POINT('Ctrl Pts',(3.12644962887386,0.353426146694047,11.6047609273293));
#14295=CARTESIAN_POINT('Ctrl Pts',(3.1803072298058,0.571644957561606,11.5916448303444));
#14296=CARTESIAN_POINT('Ctrl Pts',(3.21018867241104,0.66350393532436,11.5859441217902));
#14297=CARTESIAN_POINT('Ctrl Pts',(3.25072467712301,0.762968373975857,11.5792092606406));
#14298=CARTESIAN_POINT('Ctrl Pts',(3.25494093482936,0.773074990007728,11.5785181984935));
#14299=CARTESIAN_POINT('Ctrl Pts',(3.26145121226026,0.788325874490059,11.5774644116682));
#14300=CARTESIAN_POINT('Ctrl Pts',(3.26368423840555,0.793496176989743,11.5771052367517));
#14301=CARTESIAN_POINT('Ctrl Pts',(3.26773950774613,0.802777482404624,11.5764568884718));
#14302=CARTESIAN_POINT('Ctrl Pts',(3.26955378822361,0.806891854079918,11.5761681974725));
#14303=CARTESIAN_POINT('Ctrl Pts',(3.2735704485401,0.815917923389075,11.5755320324392));
#14304=CARTESIAN_POINT('Ctrl Pts',(3.27577877481209,0.820826790967474,11.5751842096672));
#14305=CARTESIAN_POINT('Ctrl Pts',(3.28218695193392,0.8349187408802,11.5741805311362));
#14306=CARTESIAN_POINT('Ctrl Pts',(3.28643662822085,0.844078789394303,11.5735217707392));
#14307=CARTESIAN_POINT('Ctrl Pts',(3.31775848364197,0.910270953411155,11.5687173289571));
#14308=CARTESIAN_POINT('Ctrl Pts',(3.34745253536849,0.966016114350126,11.5644334249775));
#14309=CARTESIAN_POINT('Ctrl Pts',(3.44645538127054,1.13234727732085,11.5511020071269));
#14310=CARTESIAN_POINT('Ctrl Pts',(3.52401071206225,1.23762820550267,11.5419009114411));
#14311=CARTESIAN_POINT('Ctrl Pts',(3.67110811152646,1.40103195543772,11.5268370571725));
#14312=CARTESIAN_POINT('Ctrl Pts',(3.73532700286554,1.46338692694807,11.5208451720603));
#14313=CARTESIAN_POINT('Ctrl Pts',(3.81547589695396,1.5313690984305,11.5140210918967));
#14314=CARTESIAN_POINT('Ctrl Pts',(3.82754898014606,1.54136720532858,11.5130090495106));
#14315=CARTESIAN_POINT('Ctrl Pts',(3.84755773514497,1.55754331700233,11.5113572728041));
#14316=CARTESIAN_POINT('Ctrl Pts',(3.85542431510439,1.56380531507149,11.51071418991));
#14317=CARTESIAN_POINT('Ctrl Pts',(3.86966517140209,1.57496654650411,11.5095611996311));
#14318=CARTESIAN_POINT('Ctrl Pts',(3.87602231055481,1.57988719490776,11.5090504511024));
#14319=CARTESIAN_POINT('Ctrl Pts',(3.88965379784387,1.59030727904153,11.5079635573533));
#14320=CARTESIAN_POINT('Ctrl Pts',(3.89693648090182,1.59579554911348,11.5073878566739));
#14321=CARTESIAN_POINT('Ctrl Pts',(3.91676776666068,1.61052838411179,11.5058333997876));
#14322=CARTESIAN_POINT('Ctrl Pts',(3.92938766422097,1.61967625581621,11.5048583852831));
#14323=CARTESIAN_POINT('Ctrl Pts',(3.99706719964905,1.66753565296911,11.4997020045978));
#14324=CARTESIAN_POINT('Ctrl Pts',(4.05395571379944,1.70359219421477,11.4956220633021));
#14325=CARTESIAN_POINT('Ctrl Pts',(4.25381655472482,1.81651639960299,11.4819550380108));
#14326=CARTESIAN_POINT('Ctrl Pts',(4.4042662964113,1.87878955856959,11.4728138322018));
#14327=CARTESIAN_POINT('Ctrl Pts',(4.61485900524822,1.93721170622776,11.4597980825417));
#14328=CARTESIAN_POINT('Ctrl Pts',(4.66973898160766,1.94996093511623,11.4563813201229));
#14329=CARTESIAN_POINT('Ctrl Pts',(4.73425083427601,1.96209569912148,11.4522593735123));
#14330=CARTESIAN_POINT('Ctrl Pts',(4.74343454934524,1.96375652180609,11.4516701133919));
#14331=CARTESIAN_POINT('Ctrl Pts',(4.75832176221106,1.96634103693494,11.4507104041076));
#14332=CARTESIAN_POINT('Ctrl Pts',(4.76401833455827,1.96730452194909,11.4503421104856));
#14333=CARTESIAN_POINT('Ctrl Pts',(4.774165577162,1.96897545609932,11.4496840547051));
#14334=CARTESIAN_POINT('Ctrl Pts',(4.77861455609376,1.96969258716985,11.4493948404896));
#14335=CARTESIAN_POINT('Ctrl Pts',(4.78827213971658,1.97121573475031,11.4487654923335));
#14336=CARTESIAN_POINT('Ctrl Pts',(4.79348144022065,1.97201617396001,11.4484250643612));
#14337=CARTESIAN_POINT('Ctrl Pts',(4.80816098012414,1.97421225621957,11.4474631773094));
#14338=CARTESIAN_POINT('Ctrl Pts',(4.81763802915656,1.97556036457421,11.4468391685647));
#14339=CARTESIAN_POINT('Ctrl Pts',(4.8770824348877,1.9835802337602,11.4429077395189));
#14340=CARTESIAN_POINT('Ctrl Pts',(4.92727376450225,1.98842345519148,11.4395118678819));
#14341=CARTESIAN_POINT('Ctrl Pts',(5.12402973110369,1.99990828585557,11.426032931973));
#14342=CARTESIAN_POINT('Ctrl Pts',(5.27096758985521,1.99227774766367,11.4156466494535));
#14343=CARTESIAN_POINT('Ctrl Pts',(5.5015524753863,1.95457079073536,11.3996565449744));
#14344=CARTESIAN_POINT('Ctrl Pts',(5.58635709749293,1.93494310283634,11.3938349806183));
#14345=CARTESIAN_POINT('Ctrl Pts',(5.68455797807565,1.90533673127471,11.3871758661661));
#14346=CARTESIAN_POINT('Ctrl Pts',(5.69944221329449,1.90065814625408,11.3861686296699));
#14347=CARTESIAN_POINT('Ctrl Pts',(5.72380443770009,1.89268508218576,11.3845230947587));
#14348=CARTESIAN_POINT('Ctrl Pts',(5.73331495794085,1.88949293541946,11.3838814900212));
#14349=CARTESIAN_POINT('Ctrl Pts',(5.75040028972526,1.88361457439304,11.382730144248));
#14350=CARTESIAN_POINT('Ctrl Pts',(5.75798366125667,1.88095408885977,11.3822195716927));
#14351=CARTESIAN_POINT('Ctrl Pts',(5.77415033922349,1.87517234888367,11.3811319850696));
#14352=CARTESIAN_POINT('Ctrl Pts',(5.78272872921884,1.87203781973731,11.3805554225017));
#14353=CARTESIAN_POINT('Ctrl Pts',(5.80524392747031,1.86363508144071,11.3790433712668));
#14354=CARTESIAN_POINT('Ctrl Pts',(5.81914393464503,1.85826939086074,11.3781111287979));
#14355=CARTESIAN_POINT('Ctrl Pts',(5.88756817124212,1.8309714784427,11.3735264018142));
#14356=CARTESIAN_POINT('Ctrl Pts',(5.94116779089437,1.80679168336258,11.3699498741989));
#14357=CARTESIAN_POINT('Ctrl Pts',(6.10256747418618,1.72521613558311,11.3591277120932));
#14358=CARTESIAN_POINT('Ctrl Pts',(6.20622532553586,1.66027093979745,11.3521167650349));
#14359=CARTESIAN_POINT('Ctrl Pts',(6.34356960318351,1.5555500211298,11.3420594671607));
#14360=CARTESIAN_POINT('Ctrl Pts',(6.38265443822109,1.52332395142324,11.339094760132));
#14361=CARTESIAN_POINT('Ctrl Pts',(6.46156619235591,1.45304715459529,11.3327955795476));
#14362=CARTESIAN_POINT('Ctrl Pts',(6.50112723761924,1.41476549442104,11.3294540449623));
#14363=CARTESIAN_POINT('Ctrl Pts',(6.54544682484455,1.36817907937161,11.3254159573132));
#14364=CARTESIAN_POINT('Ctrl Pts',(6.5517951725238,1.36141210190463,11.3248300556563));
#14365=CARTESIAN_POINT('Ctrl Pts',(6.56200810911264,1.35037233329508,11.3238747749475));
#14366=CARTESIAN_POINT('Ctrl Pts',(6.56590188664579,1.34612656723289,11.3235075197805));
#14367=CARTESIAN_POINT('Ctrl Pts',(6.5728075525418,1.3385308517446,11.3228506074677));
#14368=CARTESIAN_POINT('Ctrl Pts',(6.57582655010998,1.33518749606565,11.322561490991));
#14369=CARTESIAN_POINT('Ctrl Pts',(6.58236063324838,1.32790193300165,11.3219315113848));
#14370=CARTESIAN_POINT('Ctrl Pts',(6.58587134202905,1.32395604229581,11.3215903485464));
#14371=CARTESIAN_POINT('Ctrl Pts',(6.59308779257652,1.31577989505242,11.3208835978736));
#14372=CARTESIAN_POINT('Ctrl Pts',(6.59679139508719,1.31154781949649,11.3205178632326));
#14373=CARTESIAN_POINT('Ctrl Pts',(6.61545622083189,1.29003680253104,11.3186595855437));
#14374=CARTESIAN_POINT('Ctrl Pts',(6.63013687293991,1.27251809778387,11.3171484720793));
#14375=CARTESIAN_POINT('Ctrl Pts',(6.69740922142852,1.18937955789207,11.3100029078068));
#14376=CARTESIAN_POINT('Ctrl Pts',(6.74611468525271,1.12073307907979,11.3041797932713));
#14377=CARTESIAN_POINT('Ctrl Pts',(6.83249001194355,0.981071210953838,11.2927431948972));
#14378=CARTESIAN_POINT('Ctrl Pts',(6.87049712651189,0.91043614565442,11.2871429091292));
#14379=CARTESIAN_POINT('Ctrl Pts',(6.94615230437225,0.746941129047247,11.2747424973385));
#14380=CARTESIAN_POINT('Ctrl Pts',(6.98127167658435,0.653137132023966,11.2680106557683));
#14381=CARTESIAN_POINT('Ctrl Pts',(7.01368105693964,0.541705590254264,11.2604719982906));
#14382=CARTESIAN_POINT('Ctrl Pts',(7.01796762451514,0.526276951425439,11.2594378099577));
#14383=CARTESIAN_POINT('Ctrl Pts',(7.02466876595964,0.500980424685786,11.2577574519961));
#14384=CARTESIAN_POINT('Ctrl Pts',(7.0271944967768,0.491142994014301,11.2571077336037));
#14385=CARTESIAN_POINT('Ctrl Pts',(7.0315867617794,0.473476543393289,11.255947512305));
#14386=CARTESIAN_POINT('Ctrl Pts',(7.03348124097738,0.465654765531611,11.2554361234979));
#14387=CARTESIAN_POINT('Ctrl Pts',(7.03740594312717,0.449011135717347,11.2543527405092));
#14388=CARTESIAN_POINT('Ctrl Pts',(7.03942356160959,0.440186474804402,11.2537811591504));
#14389=CARTESIAN_POINT('Ctrl Pts',(7.04341203632877,0.4221783589964,11.2526203949873));
#14390=CARTESIAN_POINT('Ctrl Pts',(7.04537824427773,0.412994100472801,11.2520313717092));
#14391=CARTESIAN_POINT('Ctrl Pts',(7.0501324881265,0.389994405001584,11.250563512928));
#14392=CARTESIAN_POINT('Ctrl Pts',(7.0528391407603,0.376162528202848,11.2496872309534));
#14393=CARTESIAN_POINT('Ctrl Pts',(7.07757825008149,0.242220603678845,11.2412608649073));
#14394=CARTESIAN_POINT('Ctrl Pts',(7.08868493723875,0.120353679506743,11.2340749555492));
#14395=CARTESIAN_POINT('Ctrl Pts',(7.08857636721997,-0.00177331764829418,
11.2269712774823));
#14396=CARTESIAN_POINT('Origin',(5.09382715545311,0.,-5.29363746883395));
#14397=CARTESIAN_POINT('',(7.54432661329192,-0.00163007106614652,-5.03580997262189));
#14398=CARTESIAN_POINT('',(4.01701575109769,-2.20564845811992,-5.29358888258478));
#14399=CARTESIAN_POINT('Ctrl Pts',(7.54716444752953,-0.00163195879212374,
-5.03580997262189));
#14400=CARTESIAN_POINT('Ctrl Pts',(7.54778240942886,-0.0888794390604748,
-5.04035856840935));
#14401=CARTESIAN_POINT('Ctrl Pts',(7.50402127856605,-0.986360486250927,
-5.08718292203284));
#14402=CARTESIAN_POINT('Ctrl Pts',(6.43805680969878,-2.52634576703256,-5.17310922535387));
#14403=CARTESIAN_POINT('Ctrl Pts',(4.69254185664738,-2.5308373754473,-5.25448693288734));
#14404=CARTESIAN_POINT('Ctrl Pts',(4.01701575109769,-2.20564845811992,-5.29358888258478));
#14405=CARTESIAN_POINT('',(6.1689156158044,-2.20207516956608,-5.29363746883395));
#14406=CARTESIAN_POINT('Origin',(5.09382715545311,0.,-5.29363746883395));
#14407=CARTESIAN_POINT('',(7.54449186889422,-0.00262135351006776,-5.15146496504602));
#14408=CARTESIAN_POINT('Ctrl Pts',(6.1689156158044,-2.20207516956608,-5.29363746883395));
#14409=CARTESIAN_POINT('Ctrl Pts',(6.90007729696917,-1.84511029528062,-5.25136171099787));
#14410=CARTESIAN_POINT('Ctrl Pts',(7.497763573434,-1.00822696320923,-5.20397087640191));
#14411=CARTESIAN_POINT('Ctrl Pts',(7.54733002393177,-0.100698414309727,
-5.15658004180592));
#14412=CARTESIAN_POINT('Ctrl Pts',(7.54656647390473,-0.00262357261131683,
-5.15146496504602));
#14413=CARTESIAN_POINT('',(7.54432697499699,-0.000940433632949707,-4.35146496508883));
#14414=CARTESIAN_POINT('Ctrl Pts',(7.54432575358315,-0.0026211758248253,
-5.15146496504602));
#14415=CARTESIAN_POINT('Ctrl Pts',(7.54441040290628,0.0765162272050172,
-5.14733375399662));
#14416=CARTESIAN_POINT('Ctrl Pts',(7.54065738891893,0.155829528594839,-5.14320254294721));
#14417=CARTESIAN_POINT('Ctrl Pts',(7.53304225424233,0.234904133294203,-5.13907133189781));
#14418=CARTESIAN_POINT('Ctrl Pts',(7.52543177817542,0.313930363573951,-5.13494264814446));
#14419=CARTESIAN_POINT('Ctrl Pts',(7.51396386810591,0.392717702539037,-5.13081396439111));
#14420=CARTESIAN_POINT('Ctrl Pts',(7.49866616683113,0.470849847992309,-5.12668528063777));
#14421=CARTESIAN_POINT('Ctrl Pts',(7.48339424086519,0.548850347511155,-5.12256355336088));
#14422=CARTESIAN_POINT('Ctrl Pts',(7.4643054647924,0.626197374386007,-5.118441826084));
#14423=CARTESIAN_POINT('Ctrl Pts',(7.44147915557445,0.702481555861974,-5.11432009880711));
#14424=CARTESIAN_POINT('Ctrl Pts',(7.41866391570903,0.778728744213543,-5.11020037031382));
#14425=CARTESIAN_POINT('Ctrl Pts',(7.39211487585167,0.853913642941191,-5.10608064182052));
#14426=CARTESIAN_POINT('Ctrl Pts',(7.36196189456157,0.92763950716289,-5.10196091332722));
#14427=CARTESIAN_POINT('Ctrl Pts',(7.33181340312425,1.00135439342277,-5.09784179827159));
#14428=CARTESIAN_POINT('Ctrl Pts',(7.29806222060958,1.07361022558622,-5.09372268321596));
#14429=CARTESIAN_POINT('Ctrl Pts',(7.26088665635795,1.14402944434926,-5.08960356816033));
#14430=CARTESIAN_POINT('Ctrl Pts',(7.22356724224814,1.21472114840839,-5.08546851429842));
#14431=CARTESIAN_POINT('Ctrl Pts',(7.18279711056472,1.28356155334622,-5.08133346043652));
#14432=CARTESIAN_POINT('Ctrl Pts',(7.13880262173743,1.35019464978026,-5.07719840657462));
#14433=CARTESIAN_POINT('Ctrl Pts',(7.09492122864415,1.41665645387401,-5.07307398261124));
#14434=CARTESIAN_POINT('Ctrl Pts',(7.04783235903743,1.48092191342971,-5.06894955864786));
#14435=CARTESIAN_POINT('Ctrl Pts',(6.99780214333237,1.54266960024827,-5.06482513468448));
#14436=CARTESIAN_POINT('Ctrl Pts',(6.94757851293935,1.6046560010002,-5.06068476587332));
#14437=CARTESIAN_POINT('Ctrl Pts',(6.89439108978141,1.66410476551921,-5.05654439706216));
#14438=CARTESIAN_POINT('Ctrl Pts',(6.83854606016657,1.720728390402,-5.052404028251));
#14439=CARTESIAN_POINT('Ctrl Pts',(6.78270103055173,1.77735201528479,-5.04826365943984));
#14440=CARTESIAN_POINT('Ctrl Pts',(6.724198804172,1.83115022519108,-5.04412329062867));
#14441=CARTESIAN_POINT('Ctrl Pts',(6.66337677971777,1.88187784592164,-5.03998292181751));
#14442=CARTESIAN_POINT('Ctrl Pts',(6.60111142291994,1.93380925452955,-5.03574430030475));
#14443=CARTESIAN_POINT('Ctrl Pts',(6.53615191711457,1.98274220618099,-5.03150567879198));
#14444=CARTESIAN_POINT('Ctrl Pts',(6.46881852374267,2.02838580825473,-5.02726705727922));
#14445=CARTESIAN_POINT('Ctrl Pts',(6.40158107006867,2.07396437523705,-5.02303447514821));
#14446=CARTESIAN_POINT('Ctrl Pts',(6.33197682745093,2.11626264435325,-5.0188018930172));
#14447=CARTESIAN_POINT('Ctrl Pts',(6.2603593791009,2.15502965668488,-5.01456931088619));
#14448=CARTESIAN_POINT('Ctrl Pts',(6.18882484308392,2.1937517880062,-5.01034162886357));
#14449=CARTESIAN_POINT('Ctrl Pts',(6.11528213913476,2.22895056917049,-5.00611394684095));
#14450=CARTESIAN_POINT('Ctrl Pts',(6.04011287722191,2.26041889542105,-5.00188626481833));
#14451=CARTESIAN_POINT('Ctrl Pts',(5.96499148420126,2.29186718217835,-4.99766127504583));
#14452=CARTESIAN_POINT('Ctrl Pts',(5.88824601557778,2.31958955200984,-4.99343628527334));
#14453=CARTESIAN_POINT('Ctrl Pts',(5.8102806585679,2.34342583152839,-4.98921129550084));
#14454=CARTESIAN_POINT('Ctrl Pts',(5.73234130671429,2.36725416051357,-4.98498771496347));
#14455=CARTESIAN_POINT('Ctrl Pts',(5.65318331704386,2.38719883833571,-4.9807641344261));
#14456=CARTESIAN_POINT('Ctrl Pts',(5.57322740388629,2.40314911143737,-4.97654055388872));
#14457=CARTESIAN_POINT('Ctrl Pts',(5.49327391264045,2.41909890139586,-4.97231710128609));
#14458=CARTESIAN_POINT('Ctrl Pts',(5.41252300024027,2.43105443771684,-4.96809364868346));
#14459=CARTESIAN_POINT('Ctrl Pts',(5.33140558690961,2.43895607564111,-4.96387019608083));
#14460=CARTESIAN_POINT('Ctrl Pts',(5.2502104169818,2.44686528782658,-4.95964269500958));
#14461=CARTESIAN_POINT('Ctrl Pts',(5.16864850614162,2.45071279281044,-4.95541519393833));
#14462=CARTESIAN_POINT('Ctrl Pts',(5.08715538903955,2.45049091765975,-4.95118769286707));
#14463=CARTESIAN_POINT('Ctrl Pts',(5.00562544874515,2.45026894225334,-4.9469582815721));
#14464=CARTESIAN_POINT('Ctrl Pts',(4.92416482723625,2.44597394660128,-4.94272887027713));
#14465=CARTESIAN_POINT('Ctrl Pts',(4.84320606541023,2.43765036853641,-4.93849945898217));
#14466=CARTESIAN_POINT('Ctrl Pts',(4.76210292966866,2.42931194701879,-4.93426250536991));
#14467=CARTESIAN_POINT('Ctrl Pts',(4.68150390129521,2.41693065545801,-4.93002555175765));
#14468=CARTESIAN_POINT('Ctrl Pts',(4.60183332778805,2.40060249177982,-4.92578859814539));
#14469=CARTESIAN_POINT('Ctrl Pts',(4.52265109367718,2.38437441129724,-4.92157761486669));
#14470=CARTESIAN_POINT('Ctrl Pts',(4.44438637243818,2.36424791318695,-4.91736663158799));
#14471=CARTESIAN_POINT('Ctrl Pts',(4.36743896401488,2.340365451236,-4.9131556483093));
#14472=CARTESIAN_POINT('Ctrl Pts',(4.28997216954912,2.3163217854492,-4.90891624138405));
#14473=CARTESIAN_POINT('Ctrl Pts',(4.21356166607285,2.28838467134188,-4.9046768344588));
#14474=CARTESIAN_POINT('Ctrl Pts',(4.13862570813318,2.25666578053506,-4.90043742753356));
#14475=CARTESIAN_POINT('Ctrl Pts',(4.06379399234112,2.22499101334243,-4.8962039179758));
#14476=CARTESIAN_POINT('Ctrl Pts',(3.99043317048696,2.18954509819096,-4.89197040841805));
#14477=CARTESIAN_POINT('Ctrl Pts',(3.91894595991049,2.15048934579094,-4.8877368988603));
#14478=CARTESIAN_POINT('Ctrl Pts',(3.84753791118406,2.11147684204463,-4.88350807730822));
#14479=CARTESIAN_POINT('Ctrl Pts',(3.77799975419623,2.06886266693087,-4.87927925575614));
#14480=CARTESIAN_POINT('Ctrl Pts',(3.71071252885978,2.02285545200432,-4.87505043420406));
#14481=CARTESIAN_POINT('Ctrl Pts',(3.6434660984384,1.97687613034303,-4.87082417650292));
#14482=CARTESIAN_POINT('Ctrl Pts',(3.57846827138453,1.92750811351861,-4.86659791880178));
#14483=CARTESIAN_POINT('Ctrl Pts',(3.51607285230926,1.87500442903772,-4.86237166110065));
#14484=CARTESIAN_POINT('Ctrl Pts',(3.45369636419676,1.82251667433678,-4.85814668565914));
#14485=CARTESIAN_POINT('Ctrl Pts',(3.39392106969408,1.76689543933148,-4.85392171021764));
#14486=CARTESIAN_POINT('Ctrl Pts',(3.33706817332974,1.70843440867036,-4.84969673477613));
#14487=CARTESIAN_POINT('Ctrl Pts',(3.28021530742337,1.64997340932875,-4.84547176159809));
#14488=CARTESIAN_POINT('Ctrl Pts',(3.22628515825109,1.58867295004995,-4.84124678842004));
#14489=CARTESIAN_POINT('Ctrl Pts',(3.17556149055324,1.52486297380003,-4.83702181524199));
#14490=CARTESIAN_POINT('Ctrl Pts',(3.12478693488892,1.46098898088728,-4.83279260340568));
#14491=CARTESIAN_POINT('Ctrl Pts',(3.0772255758737,1.39460080451466,-4.82856339156937));
#14492=CARTESIAN_POINT('Ctrl Pts',(3.03311999921932,1.32606043084275,-4.82433417973306));
#14493=CARTESIAN_POINT('Ctrl Pts',(2.98899339547624,1.25748738092836,-4.82010295164349));
#14494=CARTESIAN_POINT('Ctrl Pts',(2.94832608785976,1.18676049106336,-4.81587172355392));
#14495=CARTESIAN_POINT('Ctrl Pts',(2.91131523202827,1.11426745178544,-4.81164049546435));
#14496=CARTESIAN_POINT('Ctrl Pts',(2.8742369808903,1.04164240554658,-4.80740156247558));
#14497=CARTESIAN_POINT('Ctrl Pts',(2.8408286781381,0.967245205970693,-4.8031626294868));
#14498=CARTESIAN_POINT('Ctrl Pts',(2.81123970595368,0.891484596270571,-4.79892369649802));
#14499=CARTESIAN_POINT('Ctrl Pts',(2.78193338253604,0.816447690076199,-4.79472525593237));
#14500=CARTESIAN_POINT('Ctrl Pts',(2.75637377629209,0.74007375723796,-4.79052681536673));
#14501=CARTESIAN_POINT('Ctrl Pts',(2.7346569978228,0.662771768670451,-4.78632837480108));
#14502=CARTESIAN_POINT('Ctrl Pts',(2.71279595531059,0.584956264831261,-4.7821020440946));
#14503=CARTESIAN_POINT('Ctrl Pts',(2.69474723143283,0.505908991203818,-4.77787571338812));
#14504=CARTESIAN_POINT('Ctrl Pts',(2.68064637115932,0.426038439950232,-4.77364938268164));
#14505=CARTESIAN_POINT('Ctrl Pts',(2.66656596150763,0.346283725773699,-4.7694291814658));
#14506=CARTESIAN_POINT('Ctrl Pts',(2.65642212514089,0.265708560236698,-4.76520898024995));
#14507=CARTESIAN_POINT('Ctrl Pts',(2.65030041091275,0.184735753756496,-4.7609887790341));
#14508=CARTESIAN_POINT('Ctrl Pts',(2.64416643639912,0.103600778692895,-4.75676012579489));
#14509=CARTESIAN_POINT('Ctrl Pts',(2.64207082859058,0.0220670254031271,
-4.75253147255567));
#14510=CARTESIAN_POINT('Ctrl Pts',(2.64404793261838,-0.0594307106405606,
-4.74830281931645));
#14511=CARTESIAN_POINT('Ctrl Pts',(2.6460174770955,-0.14061683623954,-4.7440903345327));
#14512=CARTESIAN_POINT('Ctrl Pts',(2.65202864769558,-0.22176675096376,-4.73987784974896));
#14513=CARTESIAN_POINT('Ctrl Pts',(2.66206332567863,-0.302448220693316,
-4.73566536496521));
#14514=CARTESIAN_POINT('Ctrl Pts',(2.67209460104101,-0.383102332451107,
-4.73145430857686));
#14515=CARTESIAN_POINT('Ctrl Pts',(2.68614661716576,-0.463287852423471,
-4.72724325218851));
#14516=CARTESIAN_POINT('Ctrl Pts',(2.70414938777136,-0.542577567401701,
-4.72303219580016));
#14517=CARTESIAN_POINT('Ctrl Pts',(2.72215160421661,-0.621864841688081,
-4.71882126903633));
#14518=CARTESIAN_POINT('Ctrl Pts',(2.74410422910218,-0.700255911458633,
-4.7146103422725));
#14519=CARTESIAN_POINT('Ctrl Pts',(2.76988644792786,-0.77733508727384,-4.71039941550866));
#14520=CARTESIAN_POINT('Ctrl Pts',(2.79585601766407,-0.854974372126607,
-4.70615788932401));
#14521=CARTESIAN_POINT('Ctrl Pts',(2.82571092881134,-0.931282159326933,
-4.70191636313936));
#14522=CARTESIAN_POINT('Ctrl Pts',(2.8592776600035,-1.00585227662211,-4.69767483695472));
#14523=CARTESIAN_POINT('Ctrl Pts',(2.89265037987298,-1.07999138837773,-4.6934578262375));
#14524=CARTESIAN_POINT('Ctrl Pts',(2.92969185937331,-1.15241247193342,-4.68924081552028));
#14525=CARTESIAN_POINT('Ctrl Pts',(2.97018535081307,-1.22274107462912,-4.68502380480306));
#14526=CARTESIAN_POINT('Ctrl Pts',(3.0110319538301,-1.29368295721111,-4.68077002088469));
#14527=CARTESIAN_POINT('Ctrl Pts',(3.05539080386526,-1.36249528115039,-4.67651623696633));
#14528=CARTESIAN_POINT('Ctrl Pts',(3.10299593847398,-1.42882515217972,-4.67226245304796));
#14529=CARTESIAN_POINT('Ctrl Pts',(3.1506010730827,-1.49515502320905,-4.6680086691296));
#14530=CARTESIAN_POINT('Ctrl Pts',(3.20145214292242,-1.55900210626518,-4.66375488521123));
#14531=CARTESIAN_POINT('Ctrl Pts',(3.25524435580459,-1.62005047416326,-4.65950110129287));
#14532=CARTESIAN_POINT('Ctrl Pts',(3.30877840952224,-1.68080585921481,-4.65526773210079));
#14533=CARTESIAN_POINT('Ctrl Pts',(3.3654266037922,-1.73901772985628,-4.65103436290872));
#14534=CARTESIAN_POINT('Ctrl Pts',(3.42491790165664,-1.79435006411583,-4.64680099371664));
#14535=CARTESIAN_POINT('Ctrl Pts',(3.48432428573454,-1.84960342080744,-4.64257366694456));
#14536=CARTESIAN_POINT('Ctrl Pts',(3.54656537632463,-1.90198509065237,-4.63834634017248));
#14537=CARTESIAN_POINT('Ctrl Pts',(3.61133105720728,-1.9511933703982,-4.6341190134004));
#14538=CARTESIAN_POINT('Ctrl Pts',(3.67608993510763,-2.00039648130999,-4.62989213066641));
#14539=CARTESIAN_POINT('Ctrl Pts',(3.74337254318219,-2.04642653984645,-4.62566524793242));
#14540=CARTESIAN_POINT('Ctrl Pts',(3.81283321839339,-2.08902005333032,-4.62143836519843));
#14541=CARTESIAN_POINT('Ctrl Pts',(3.88217701172922,-2.13154189446551,-4.61721859506419));
#14542=CARTESIAN_POINT('Ctrl Pts',(3.95369116722407,-2.17063848015603,-4.61299882492994));
#14543=CARTESIAN_POINT('Ctrl Pts',(4.02700158347371,-2.20609008178968,-4.6087790547957));
#14544=CARTESIAN_POINT('Ctrl Pts',(4.10028795109302,-2.2415300539373,-4.60456066890802));
#14545=CARTESIAN_POINT('Ctrl Pts',(4.17536899153297,-2.27332721461545,-4.60034228302035));
#14546=CARTESIAN_POINT('Ctrl Pts',(4.25184670815908,-2.30130814459397,-4.59612389713267));
#14547=CARTESIAN_POINT('Ctrl Pts',(4.32832269787782,-2.32928844274826,-4.59190560649838));
#14548=CARTESIAN_POINT('Ctrl Pts',(4.4061948645903,-2.3534525230627,-4.58768731586409));
#14549=CARTESIAN_POINT('Ctrl Pts',(4.48504732199531,-2.37367591814365,-4.58346902522981));
#14550=CARTESIAN_POINT('Ctrl Pts',(4.56417349122223,-2.39396951246119,-4.57923609210938));
#14551=CARTESIAN_POINT('Ctrl Pts',(4.64428631532835,-2.41029489064329,-4.57500315898895));
#14552=CARTESIAN_POINT('Ctrl Pts',(4.72495420216572,-2.42257775816031,-4.57077022586852));
#14553=CARTESIAN_POINT('Ctrl Pts',(4.80545917820924,-2.4348358201224,-4.56654584126128));
#14554=CARTESIAN_POINT('Ctrl Pts',(4.88651650907397,-2.44306767202367,-4.56232145665404));
#14555=CARTESIAN_POINT('Ctrl Pts',(4.96769285381683,-2.44725159882484,-4.55809707204681));
#14556=CARTESIAN_POINT('Ctrl Pts',(5.04911560263457,-2.45144822558948,-4.55385986466978));
#14557=CARTESIAN_POINT('Ctrl Pts',(5.13065761996133,-2.45157232879408,-4.54962265729275));
#14558=CARTESIAN_POINT('Ctrl Pts',(5.21188426209025,-2.44765454457374,-4.54538544991573));
#14559=CARTESIAN_POINT('Ctrl Pts',(5.29311090421916,-2.44373676035339,-4.5411482425387));
#14560=CARTESIAN_POINT('Ctrl Pts',(5.37402171465691,-2.43577719546714,-4.53691103516168));
#14561=CARTESIAN_POINT('Ctrl Pts',(5.45419165970096,-2.42385801442209,-4.53267382778465));
#14562=CARTESIAN_POINT('Ctrl Pts',(5.53428105576291,-2.41195080891102,-4.52844087764818));
#14563=CARTESIAN_POINT('Ctrl Pts',(5.61392832466803,-2.39604775380258,-4.5242079275117));
#14564=CARTESIAN_POINT('Ctrl Pts',(5.69270415841357,-2.37619371797105,-4.51997497737523));
#14565=CARTESIAN_POINT('Ctrl Pts',(5.77136778124399,-2.35636796288787,-4.51574805679358));
#14566=CARTESIAN_POINT('Ctrl Pts',(5.84916198766149,-2.33260251745521,-4.51152113621193));
#14567=CARTESIAN_POINT('Ctrl Pts',(5.92566503819675,-2.30499370646268,-4.50729421563028));
#14568=CARTESIAN_POINT('Ctrl Pts',(6.00216927074345,-2.27738446889985,-4.50306722974054));
#14569=CARTESIAN_POINT('Ctrl Pts',(6.07738185167261,-2.24593184421965,-4.4988402438508));
#14570=CARTESIAN_POINT('Ctrl Pts',(6.15089365509811,-2.21078281731342,-4.49461325796105));
#14571=CARTESIAN_POINT('Ctrl Pts',(6.22427350784327,-2.1756968814728,-4.49039385933809));
#14572=CARTESIAN_POINT('Ctrl Pts',(6.29595825306512,-2.13692797762798,-4.48617446071512));
#14573=CARTESIAN_POINT('Ctrl Pts',(6.36556019118147,-2.09467069866295,-4.48195506209215));
#14574=CARTESIAN_POINT('Ctrl Pts',(6.43513952610997,-2.05242714272403,-4.47773703371637));
#14575=CARTESIAN_POINT('Ctrl Pts',(6.50263700048167,-2.00669770229264,-4.47351900534059));
#14576=CARTESIAN_POINT('Ctrl Pts',(6.56769080516089,-1.95772219481469,-4.4693009769648));
#14577=CARTESIAN_POINT('Ctrl Pts',(6.63274336537986,-1.90874762422387,-4.46508302927867));
#14578=CARTESIAN_POINT('Ctrl Pts',(6.69535197849001,-1.85652739034329,-4.46086508159254));
#14579=CARTESIAN_POINT('Ctrl Pts',(6.75518620855875,-1.80134292866848,-4.4566471339064));
#14580=CARTESIAN_POINT('Ctrl Pts',(6.81523937887182,-1.74595654078005,-4.45241375227057));
#14581=CARTESIAN_POINT('Ctrl Pts',(6.87249747229355,-1.68758450384207,-4.44818037063474));
#14582=CARTESIAN_POINT('Ctrl Pts',(6.92666347913855,-1.62654888047646,-4.44394698899891));
#14583=CARTESIAN_POINT('Ctrl Pts',(6.98071048701252,-1.5656473481543,-4.43972290780976));
#14584=CARTESIAN_POINT('Ctrl Pts',(7.03167871727176,-1.50209430841,-4.43549882662062));
#14585=CARTESIAN_POINT('Ctrl Pts',(7.0793145170224,-1.43624168824353,-4.43127474543147));
#14586=CARTESIAN_POINT('Ctrl Pts',(7.12710764124051,-1.37017157979193,-4.4270367135723));
#14587=CARTESIAN_POINT('Ctrl Pts',(7.17154604090554,-1.30178707661587,-4.42279868171313));
#14588=CARTESIAN_POINT('Ctrl Pts',(7.21241914666087,-1.23146994473692,-4.41856064985395));
#14589=CARTESIAN_POINT('Ctrl Pts',(7.25329225241619,-1.16115281285797,-4.41432261799478));
#14590=CARTESIAN_POINT('Ctrl Pts',(7.29059990576516,-1.08890349424344,-4.41008458613561));
#14591=CARTESIAN_POINT('Ctrl Pts',(7.32418007214676,-1.01512369541655,-4.40584655427644));
#14592=CARTESIAN_POINT('Ctrl Pts',(7.36071056800757,-0.934861656061826,
-4.40123617195938));
#14593=CARTESIAN_POINT('Ctrl Pts',(7.3929488423299,-0.852528880741258,-4.39662578964233));
#14594=CARTESIAN_POINT('Ctrl Pts',(7.42067706440021,-0.76858295013151,-4.39201540732527));
#14595=CARTESIAN_POINT('Ctrl Pts',(7.44833404735281,-0.684852692709086,
-4.38741686996415));
#14596=CARTESIAN_POINT('Ctrl Pts',(7.47150395187169,-0.599517840836609,
-4.38281833260303));
#14597=CARTESIAN_POINT('Ctrl Pts',(7.49001655380418,-0.513056154070835,
-4.37821979524192));
#14598=CARTESIAN_POINT('Ctrl Pts',(7.5084493995364,-0.426966962518323,-4.37364106935128));
#14599=CARTESIAN_POINT('Ctrl Pts',(7.5222648532601,-0.339760926393879,-4.36906234346064));
#14600=CARTESIAN_POINT('Ctrl Pts',(7.53134271997225,-0.251928804877392,
-4.36448361757));
#14601=CARTESIAN_POINT('Ctrl Pts',(7.53994639377573,-0.168684696216461,
-4.36014406674294));
#14602=CARTESIAN_POINT('Ctrl Pts',(7.54429476187688,-0.0848785683972825,
-4.35580451591589));
#14603=CARTESIAN_POINT('Ctrl Pts',(7.54432697499699,-0.000940433632964154,
-4.35146496508883));
#14604=CARTESIAN_POINT('',(7.54432616501525,0.00220321015066406,-3.55146496500219));
#14605=CARTESIAN_POINT('Ctrl Pts',(7.54432697499731,-0.000940432804910453,
-4.35146496504602));
#14606=CARTESIAN_POINT('Ctrl Pts',(7.54435894273178,0.0823583708330137,
-4.34715846725177));
#14607=CARTESIAN_POINT('Ctrl Pts',(7.54013925399136,0.165631372021684,-4.34285196945752));
#14608=CARTESIAN_POINT('Ctrl Pts',(7.53170205545692,0.248427498339918,-4.33854547166327));
#14609=CARTESIAN_POINT('Ctrl Pts',(7.52325973533066,0.331273883990137,-4.3342363597165));
#14610=CARTESIAN_POINT('Ctrl Pts',(7.51059485692861,0.413642384925573,-4.32992724776972));
#14611=CARTESIAN_POINT('Ctrl Pts',(7.49379316422016,0.495089291706826,-4.32561813582295));
#14612=CARTESIAN_POINT('Ctrl Pts',(7.47696332659815,0.576672632131393,-4.32130180558066));
#14613=CARTESIAN_POINT('Ctrl Pts',(7.45598292601234,0.657330867510103,-4.31698547533837));
#14614=CARTESIAN_POINT('Ctrl Pts',(7.43098837314364,0.736632671365669,-4.31266914509608));
#14615=CARTESIAN_POINT('Ctrl Pts',(7.40597114511374,0.81600641814397,-4.30834889906123));
#14616=CARTESIAN_POINT('Ctrl Pts',(7.37693266243305,0.894020873270854,-4.30402865302639));
#14617=CARTESIAN_POINT('Ctrl Pts',(7.34405767683324,0.97026431999188,-4.29970840699154));
#14618=CARTESIAN_POINT('Ctrl Pts',(7.31111461608832,1.04666564613413,-4.29537921490333));
#14619=CARTESIAN_POINT('Ctrl Pts',(7.27431937545136,1.12128824639635,-4.29105002281511));
#14620=CARTESIAN_POINT('Ctrl Pts',(7.23390291427382,1.19374452732064,-4.28672083072689));
#14621=CARTESIAN_POINT('Ctrl Pts',(7.20993621035855,1.23671064016474,-4.28415364740734));
#14622=CARTESIAN_POINT('Ctrl Pts',(7.1846969767331,1.27891552146937,-4.28158646408778));
#14623=CARTESIAN_POINT('Ctrl Pts',(7.15824028834326,1.32028355543447,-4.27901928076822));
#14624=CARTESIAN_POINT('Ctrl Pts',(7.11462301567452,1.38848410988927,-4.27478694703129));
#14625=CARTESIAN_POINT('Ctrl Pts',(7.06754118317403,1.45464801911065,-4.27055461329436));
#14626=CARTESIAN_POINT('Ctrl Pts',(7.01721112668303,1.51840190635281,-4.26632227955743));
#14627=CARTESIAN_POINT('Ctrl Pts',(6.96695297675965,1.58206470839609,-4.26209599255704));
#14628=CARTESIAN_POINT('Ctrl Pts',(6.91345610538469,1.64332396541314,-4.25786970555666));
#14629=CARTESIAN_POINT('Ctrl Pts',(6.85698071948308,1.70183423389248,-4.25364341855628));
#14630=CARTESIAN_POINT('Ctrl Pts',(6.80049390648484,1.76035634120181,-4.24941627641893));
#14631=CARTESIAN_POINT('Ctrl Pts',(6.74102764743151,1.81612796965853,-4.24518913428159));
#14632=CARTESIAN_POINT('Ctrl Pts',(6.67888340738122,1.86883571461581,-4.24096199214424));
#14633=CARTESIAN_POINT('Ctrl Pts',(6.61686286860303,1.92143854212467,-4.23674326434843));
#14634=CARTESIAN_POINT('Ctrl Pts',(6.55217533763354,1.97098935202897,-4.23252453655261));
#14635=CARTESIAN_POINT('Ctrl Pts',(6.48515680212753,2.01721393617158,-4.22830580875679));
#14636=CARTESIAN_POINT('Ctrl Pts',(6.41816023415074,2.06342336868643,-4.22408846378776));
#14637=CARTESIAN_POINT('Ctrl Pts',(6.34883456118247,2.10630847704602,-4.21987111881873));
#14638=CARTESIAN_POINT('Ctrl Pts',(6.27754646223391,2.14563716707983,-4.21565377384969));
#14639=CARTESIAN_POINT('Ctrl Pts',(6.20625992476307,2.18496499566729,-4.21143652125639));
#14640=CARTESIAN_POINT('Ctrl Pts',(6.13301145415542,2.22073633738107,-4.20721926866309));
#14641=CARTESIAN_POINT('Ctrl Pts',(6.05819288644913,2.25276474290604,-4.20300201606979));
#14642=CARTESIAN_POINT('Ctrl Pts',(5.98307423198179,2.28492160986472,-4.19876784866897));
#14643=CARTESIAN_POINT('Ctrl Pts',(5.90637328831448,2.3133052574162,-4.19453368126816));
#14644=CARTESIAN_POINT('Ctrl Pts',(5.82850574459439,2.33777621269816,-4.19029951386734));
#14645=CARTESIAN_POINT('Ctrl Pts',(5.75083687156058,2.36218473296231,-4.18607614949052));
#14646=CARTESIAN_POINT('Ctrl Pts',(5.67200780663635,2.3827004234283,-4.1818527851137));
#14647=CARTESIAN_POINT('Ctrl Pts',(5.59244332756941,2.39923574558735,-4.17762942073688));
#14648=CARTESIAN_POINT('Ctrl Pts',(5.51257356926303,2.41583451176855,-4.17338985182407));
#14649=CARTESIAN_POINT('Ctrl Pts',(5.4319632089515,2.42842224104266,-4.16915028291125));
#14650=CARTESIAN_POINT('Ctrl Pts',(5.35104733214227,2.43696287019396,-4.16491071399844));
#14651=CARTESIAN_POINT('Ctrl Pts',(5.27013145533303,2.44550349934527,-4.16067114508563));
#14652=CARTESIAN_POINT('Ctrl Pts',(5.18891053157333,2.44999706458279,-4.15643157617281));
#14653=CARTESIAN_POINT('Ctrl Pts',(5.10781798867477,2.45046006018987,-4.15219200726));
#14654=CARTESIAN_POINT('Ctrl Pts',(5.02686672608006,2.45092224916102,-4.14795982456992));
#14655=CARTESIAN_POINT('Ctrl Pts',(4.94574161710686,2.44736963799979,-4.14372764187984));
#14656=CARTESIAN_POINT('Ctrl Pts',(4.8648736273461,2.4397808368719,-4.13949545918977));
#14657=CARTESIAN_POINT('Ctrl Pts',(4.78412116947314,2.43220287746919,-4.13526932279882));
#14658=CARTESIAN_POINT('Ctrl Pts',(4.70362556001836,2.42060022365766,-4.13104318640786));
#14659=CARTESIAN_POINT('Ctrl Pts',(4.62381816784454,2.40500349304677,-4.12681705001691));
#14660=CARTESIAN_POINT('Ctrl Pts',(4.54399107084123,2.38940291152798,-4.12258987017253));
#14661=CARTESIAN_POINT('Ctrl Pts',(4.46485299712538,2.36980630484773,-4.11836269032815));
#14662=CARTESIAN_POINT('Ctrl Pts',(4.38683090851581,2.34629634889043,-4.11413551048377));
#14663=CARTESIAN_POINT('Ctrl Pts',(4.30896756011833,2.32283422522603,-4.10991693106828));
#14664=CARTESIAN_POINT('Ctrl Pts',(4.23221611240439,2.29547477038324,-4.10569835165279));
#14665=CARTESIAN_POINT('Ctrl Pts',(4.15698933680047,2.26435093383119,-4.1014797722373));
#14666=CARTESIAN_POINT('Ctrl Pts',(4.08178719900443,2.23323729076542,-4.09726257446483));
#14667=CARTESIAN_POINT('Ctrl Pts',(4.00810917068676,2.19836189190233,-4.09304537669236));
#14668=CARTESIAN_POINT('Ctrl Pts',(3.93634935778715,2.15990634007828,-4.08882817891988));
#14669=CARTESIAN_POINT('Ctrl Pts',(3.8645910930412,2.12145161789831,-4.08461107212968));
#14670=CARTESIAN_POINT('Ctrl Pts',(3.79475137044941,2.07941711682518,-4.08039396533947));
#14671=CARTESIAN_POINT('Ctrl Pts',(3.72719965800537,2.03403036683815,-4.07617685854926));
#14672=CARTESIAN_POINT('Ctrl Pts',(3.65937183564308,1.98845810368831,-4.07194251481613));
#14673=CARTESIAN_POINT('Ctrl Pts',(3.59385116518287,1.93950638283866,-4.06770817108301));
#14674=CARTESIAN_POINT('Ctrl Pts',(3.53098072628333,1.88744835395071,-4.06347382734989));
#14675=CARTESIAN_POINT('Ctrl Pts',(3.46827539746185,1.83552703963584,-4.05925060383219));
#14676=CARTESIAN_POINT('Ctrl Pts',(3.4082067148203,1.78051605822941,-4.05502738031449));
#14677=CARTESIAN_POINT('Ctrl Pts',(3.35107902672125,1.72272435688406,-4.05080415679679));
#14678=CARTESIAN_POINT('Ctrl Pts',(3.29372570332407,1.66470439760992,-4.04656425295595));
#14679=CARTESIAN_POINT('Ctrl Pts',(3.23933696170591,1.60388206453133,-4.04232434911512));
#14680=CARTESIAN_POINT('Ctrl Pts',(3.18817963229373,1.54060305318291,-4.03808444527428));
#14681=CARTESIAN_POINT('Ctrl Pts',(3.13702230288155,1.47732404183449,-4.03384454143345));
#14682=CARTESIAN_POINT('Ctrl Pts',(3.08909661061961,1.41158876630477,-4.02960463759262));
#14683=CARTESIAN_POINT('Ctrl Pts',(3.04462434790387,1.34377010814064,-4.02536473375178));
#14684=CARTESIAN_POINT('Ctrl Pts',(3.00023531020732,1.2760783652442,-4.02113276443141));
#14685=CARTESIAN_POINT('Ctrl Pts',(2.95912113831476,1.20605844695567,-4.01690079511104));
#14686=CARTESIAN_POINT('Ctrl Pts',(2.92153406644567,1.13406039762022,-4.01266882579066));
#14687=CARTESIAN_POINT('Ctrl Pts',(2.88400073372037,1.0621652856335,-4.00844290701896));
#14688=CARTESIAN_POINT('Ctrl Pts',(2.84998469879711,0.988298068178758,-4.00421698824726));
#14689=CARTESIAN_POINT('Ctrl Pts',(2.81969476619186,0.912837403984379,-3.99999106947556));
#14690=CARTESIAN_POINT('Ctrl Pts',(2.78939540850371,0.837353259281616,-3.99576383575756));
#14691=CARTESIAN_POINT('Ctrl Pts',(2.76282470604432,0.760275080275662,-3.99153660203956));
#14692=CARTESIAN_POINT('Ctrl Pts',(2.74014540541728,0.682006209317958,-3.98730936832156));
#14693=CARTESIAN_POINT('Ctrl Pts',(2.71751375000239,0.60390176745901,-3.98309101527633));
#14694=CARTESIAN_POINT('Ctrl Pts',(2.69875731585562,0.524612070978461,-3.97887266223109));
#14695=CARTESIAN_POINT('Ctrl Pts',(2.68398890655482,0.444555805435994,-3.97465430918585));
#14696=CARTESIAN_POINT('Ctrl Pts',(2.66922534417337,0.364525813966359,-3.97043734058335));
#14697=CARTESIAN_POINT('Ctrl Pts',(2.65844729162773,0.283730209711626,-3.96622037198085));
#14698=CARTESIAN_POINT('Ctrl Pts',(2.65171656970815,0.202598462463126,-3.96200340337834));
#14699=CARTESIAN_POINT('Ctrl Pts',(2.6449859969881,0.121468513657372,-3.95778652825314));
#14700=CARTESIAN_POINT('Ctrl Pts',(2.6423026137912,0.0400028998962365,-3.95356965312794));
#14701=CARTESIAN_POINT('Ctrl Pts',(2.64367629924461,-0.0413646203990808,
-3.94935277800273));
#14702=CARTESIAN_POINT('Ctrl Pts',(2.64505576193407,-0.123074343758934,
-3.94511816818947));
#14703=CARTESIAN_POINT('Ctrl Pts',(2.65052649774286,-0.204684674653923,
-3.9408835583762));
#14704=CARTESIAN_POINT('Ctrl Pts',(2.6600457322559,-0.285759049025847,-3.93664894856294));
#14705=CARTESIAN_POINT('Ctrl Pts',(2.66953884154435,-0.366610917456189,
-3.93242596049639));
#14706=CARTESIAN_POINT('Ctrl Pts',(2.68305813794157,-0.446929313110711,
-3.92820297242984));
#14707=CARTESIAN_POINT('Ctrl Pts',(2.70050975822739,-0.526290875977058,
-3.92397998436328));
#14708=CARTESIAN_POINT('Ctrl Pts',(2.71803341931967,-0.605980045730181,
-3.91973956367667));
#14709=CARTESIAN_POINT('Ctrl Pts',(2.73952180815708,-0.684704012986985,
-3.91549914299005));
#14710=CARTESIAN_POINT('Ctrl Pts',(2.7648297406262,-0.762050714670325,-3.91125872230343));
#14711=CARTESIAN_POINT('Ctrl Pts',(2.79013767309531,-0.839397416353665,
-3.90701830161681));
#14712=CARTESIAN_POINT('Ctrl Pts',(2.81926492367267,-0.915366438150804,
-3.90277788093019));
#14713=CARTESIAN_POINT('Ctrl Pts',(2.85201897448302,-0.989568759478377,
-3.89853746024357));
#14714=CARTESIAN_POINT('Ctrl Pts',(2.88470900689497,-1.06362605099587,-3.89430532753765));
#14715=CARTESIAN_POINT('Ctrl Pts',(2.92113363261499,-1.1361998701706,-3.89007319483172));
#14716=CARTESIAN_POINT('Ctrl Pts',(2.96113610813775,-1.2068882080379,-3.8858410621258));
#14717=CARTESIAN_POINT('Ctrl Pts',(3.00108141513979,-1.27747552346457,-3.88161497766472));
#14718=CARTESIAN_POINT('Ctrl Pts',(3.04459418963606,-1.34618230829652,-3.87738889320364));
#14719=CARTESIAN_POINT('Ctrl Pts',(3.09147006458376,-1.41262745642482,-3.87316280874256));
#14720=CARTESIAN_POINT('Ctrl Pts',(3.13835823086516,-1.47909002715032,-3.86893561615893));
#14721=CARTESIAN_POINT('Ctrl Pts',(3.1886110488955,-1.5432893594117,-3.8647084235753));
#14722=CARTESIAN_POINT('Ctrl Pts',(3.24197843702879,-1.60486964394938,-3.86048123099166));
#14723=CARTESIAN_POINT('Ctrl Pts',(3.29523637498116,-1.66632363463009,-3.85626270787845));
#14724=CARTESIAN_POINT('Ctrl Pts',(3.3515958351206,-1.72516894203193,-3.85204418476524));
#14725=CARTESIAN_POINT('Ctrl Pts',(3.41076667511244,-1.78108328539556,-3.84782566165203));
#14726=CARTESIAN_POINT('Ctrl Pts',(3.4699181141398,-1.83697929553644,-3.84360852171028));
#14727=CARTESIAN_POINT('Ctrl Pts',(3.53187876493583,-1.88994593120588,-3.83939138176853));
#14728=CARTESIAN_POINT('Ctrl Pts',(3.59632172180472,-1.93969784404519,-3.83517424182678));
#14729=CARTESIAN_POINT('Ctrl Pts',(3.66076326611745,-1.98944866634839,-3.83095719432255));
#14730=CARTESIAN_POINT('Ctrl Pts',(3.72768663980081,-2.03598462286909,-3.82674014681832));
#14731=CARTESIAN_POINT('Ctrl Pts',(3.7967331044691,-2.07906163278097,-3.82252309931408));
#14732=CARTESIAN_POINT('Ctrl Pts',(3.86606383822575,-2.12231599373314,-3.81828868993252));
#14733=CARTESIAN_POINT('Ctrl Pts',(3.93753478830691,-2.16208260581578,-3.81405428055096));
#14734=CARTESIAN_POINT('Ctrl Pts',(4.01075634507282,-2.19816011011532,-3.8098198711694));
#14735=CARTESIAN_POINT('Ctrl Pts',(4.08378339864932,-2.23414177939082,-3.80559670992522));
#14736=CARTESIAN_POINT('Ctrl Pts',(4.15855132473493,-2.26645376745094,-3.80137354868105));
#14737=CARTESIAN_POINT('Ctrl Pts',(4.23465372403717,-2.29494471932309,-3.79715038743687));
#14738=CARTESIAN_POINT('Ctrl Pts',(4.31106016462263,-2.32354949711463,-3.79291035398661));
#14739=CARTESIAN_POINT('Ctrl Pts',(4.38881131177301,-2.34830250896049,-3.78867032053636));
#14740=CARTESIAN_POINT('Ctrl Pts',(4.46748251991742,-2.3691016541161,-3.78443028708611));
#14741=CARTESIAN_POINT('Ctrl Pts',(4.54615372806182,-2.38990079927172,-3.78019025363585));
#14742=CARTESIAN_POINT('Ctrl Pts',(4.62574452720736,-2.40674604182972,-3.7759502201856));
#14743=CARTESIAN_POINT('Ctrl Pts',(4.70582388447254,-2.41958750858661,-3.77171018673535));
#14744=CARTESIAN_POINT('Ctrl Pts',(4.78575337376834,-2.43240494262631,-3.76747808847869));
#14745=CARTESIAN_POINT('Ctrl Pts',(4.86646775907577,-2.44128140272402,-3.76324599022204));
#14746=CARTESIAN_POINT('Ctrl Pts',(4.94754441563542,-2.44612992501041,-3.75901389196539));
#14747=CARTESIAN_POINT('Ctrl Pts',(5.0285051998481,-2.4509715179329,-3.75478784209773));
#14748=CARTESIAN_POINT('Ctrl Pts',(5.10982676702841,-2.45179657878863,-3.75056179223008));
#14749=CARTESIAN_POINT('Ctrl Pts',(5.19107814952758,-2.44856947913502,-3.74633574236243));
#14750=CARTESIAN_POINT('Ctrl Pts',(5.27235166817822,-2.44534150028939,-3.74210854114845));
#14751=CARTESIAN_POINT('Ctrl Pts',(5.35355449950888,-2.43805910516314,-3.73788133993448));
#14752=CARTESIAN_POINT('Ctrl Pts',(5.43425204553073,-2.42673878780054,-3.73365413872051));
#14753=CARTESIAN_POINT('Ctrl Pts',(5.51478326397327,-2.415441803006,-3.72943565028878));
#14754=CARTESIAN_POINT('Ctrl Pts',(5.59481081425696,-2.40012356446573,-3.72521716185704));
#14755=CARTESIAN_POINT('Ctrl Pts',(5.67390647757363,-2.38085241668781,-3.7209986734253));
#14756=CARTESIAN_POINT('Ctrl Pts',(5.75297620761036,-2.36158758738614,-3.71678156811922));
#14757=CARTESIAN_POINT('Ctrl Pts',(5.83111420632424,-2.33837253259868,-3.71256446281314));
#14758=CARTESIAN_POINT('Ctrl Pts',(5.90790327031475,-2.31132653020117,-3.70834735750706));
#14759=CARTESIAN_POINT('Ctrl Pts',(5.98469065282652,-2.28428112004005,-3.70413034454451));
#14760=CARTESIAN_POINT('Ctrl Pts',(6.06012872143133,-2.25340508451674,-3.69991333158195));
#14761=CARTESIAN_POINT('Ctrl Pts',(6.13381760719522,-2.21886685276184,-3.6956963186194));
#14762=CARTESIAN_POINT('Ctrl Pts',(6.2078111989167,-2.18418580428673,-3.69146186817004));
#14763=CARTESIAN_POINT('Ctrl Pts',(6.28004067851953,-2.14581239714357,-3.68722741772069));
#14764=CARTESIAN_POINT('Ctrl Pts',(6.35012523492125,-2.10396420728221,-3.68299296727133));
#14765=CARTESIAN_POINT('Ctrl Pts',(6.42002238126497,-2.06222792184162,-3.67876983998139));
#14766=CARTESIAN_POINT('Ctrl Pts',(6.48778569490334,-2.01703570717693,-3.67454671269144));
#14767=CARTESIAN_POINT('Ctrl Pts',(6.55306723010677,-1.96864640159801,-3.67032358540149));
#14768=CARTESIAN_POINT('Ctrl Pts',(6.61861131715112,-1.92006248201038,-3.66608347337243));
#14769=CARTESIAN_POINT('Ctrl Pts',(6.68165326235673,-1.86825600696615,-3.66184336134337));
#14770=CARTESIAN_POINT('Ctrl Pts',(6.7418765192365,-1.81352792769595,-3.65760324931431));
#14771=CARTESIAN_POINT('Ctrl Pts',(6.80209977611626,-1.75879984842576,-3.65336313728525));
#14772=CARTESIAN_POINT('Ctrl Pts',(6.85950405901539,-1.70115053996431,-3.64912302525619));
#14773=CARTESIAN_POINT('Ctrl Pts',(6.91381319174004,-1.64091470763126,-3.64488291322713));
#14774=CARTESIAN_POINT('Ctrl Pts',(6.96744889663614,-1.58142579361072,-3.64069537816429));
#14775=CARTESIAN_POINT('Ctrl Pts',(7.01827548563093,-1.51918136726743,-3.63650784310144));
#14776=CARTESIAN_POINT('Ctrl Pts',(7.06599272976734,-1.45448038745451,-3.6323203080386));
#14777=CARTESIAN_POINT('Ctrl Pts',(7.11364716653421,-1.38986456969197,-3.62813828477903));
#14778=CARTESIAN_POINT('Ctrl Pts',(7.15820009761142,-1.32279899075967,-3.62395626151945));
#14779=CARTESIAN_POINT('Ctrl Pts',(7.19938935174628,-1.25361799904958,-3.61977423825987));
#14780=CARTESIAN_POINT('Ctrl Pts',(7.24053763994745,-1.18450581324478,-3.61559637434941));
#14781=CARTESIAN_POINT('Ctrl Pts',(7.27832864812245,-1.11328279551133,-3.61141851043894));
#14782=CARTESIAN_POINT('Ctrl Pts',(7.31254254993978,-1.04031353363678,-3.60724064652848));
#14783=CARTESIAN_POINT('Ctrl Pts',(7.34673342380052,-0.967393384342382,
-3.60306559456472));
#14784=CARTESIAN_POINT('Ctrl Pts',(7.37735177037304,-0.892729753487568,
-3.59889054260097));
#14785=CARTESIAN_POINT('Ctrl Pts',(7.40422367905159,-0.816711793562492,
-3.59471549063722));
#14786=CARTESIAN_POINT('Ctrl Pts',(7.43109295563704,-0.740701279567287,
-3.5905408476182));
#14787=CARTESIAN_POINT('Ctrl Pts',(7.45421635246627,-0.663337143335558,
-3.58636620459918));
#14788=CARTESIAN_POINT('Ctrl Pts',(7.47346857573817,-0.585027316339761,
-3.58219156158016));
#14789=CARTESIAN_POINT('Ctrl Pts',(7.49271959413475,-0.506722390262485,
-3.57801717982573));
#14790=CARTESIAN_POINT('Ctrl Pts',(7.50809981464966,-0.427472354483196,
-3.57384279807131));
#14791=CARTESIAN_POINT('Ctrl Pts',(7.51953466705069,-0.347697164467993,
-3.56966841631688));
#14792=CARTESIAN_POINT('Ctrl Pts',(7.53097725174323,-0.267868030160116,
-3.56549121182934));
#14793=CARTESIAN_POINT('Ctrl Pts',(7.53846908510302,-0.187513504758057,
-3.56131400734179));
#14794=CARTESIAN_POINT('Ctrl Pts',(7.54198738670963,-0.107059479234764,
-3.55713680285424));
#14795=CARTESIAN_POINT('Ctrl Pts',(7.54357977831448,-0.0706457975370414,
-3.5552461902515));
#14796=CARTESIAN_POINT('Ctrl Pts',(7.54435890520333,-0.0342117587869815,
-3.55335557764875));
#14797=CARTESIAN_POINT('Ctrl Pts',(7.54432616501601,0.00220320930666846,
-3.55146496504601));
#14798=CARTESIAN_POINT('',(7.54432706806737,-0.00065442915052629,-2.75146496500916));
#14799=CARTESIAN_POINT('Ctrl Pts',(7.54432616501525,0.00220321015066411,
-3.55146496500219));
#14800=CARTESIAN_POINT('Ctrl Pts',(7.54422973877529,0.109452355430954,-3.54589674412165));
#14801=CARTESIAN_POINT('Ctrl Pts',(7.53708802522586,0.216389416064109,-3.54032852324111));
#14802=CARTESIAN_POINT('Ctrl Pts',(7.52304979359998,0.322222941943559,-3.53476030236056));
#14803=CARTESIAN_POINT('Ctrl Pts',(7.5090115619741,0.428056467823009,-3.52919208148001));
#14804=CARTESIAN_POINT('Ctrl Pts',(7.48807700934417,0.532786801311883,-3.52362386059947));
#14805=CARTESIAN_POINT('Ctrl Pts',(7.46044938516695,0.635648858902682,-3.51805563971892));
#14806=CARTESIAN_POINT('Ctrl Pts',(7.43945115538403,0.71382862229388,-3.51382354285884));
#14807=CARTESIAN_POINT('Ctrl Pts',(7.41453567224234,0.79111260584736,-3.50959144599877));
#14808=CARTESIAN_POINT('Ctrl Pts',(7.38579644879979,0.867079585941174,-3.50535934913869));
#14809=CARTESIAN_POINT('Ctrl Pts',(7.35709829995641,0.942937992702671,-3.50113330086523));
#14810=CARTESIAN_POINT('Ctrl Pts',(7.32458742785988,1.01748270343279,-3.49690725259176));
#14811=CARTESIAN_POINT('Ctrl Pts',(7.28840760261012,1.09030587953846,-3.4926812043183));
#14812=CARTESIAN_POINT('Ctrl Pts',(7.25221790366536,1.16314892953311,-3.48845400273048));
#14813=CARTESIAN_POINT('Ctrl Pts',(7.21235739531423,1.23426906193182,-3.48422680114266));
#14814=CARTESIAN_POINT('Ctrl Pts',(7.16901889560869,1.30327644480749,-3.47999959955485));
#14815=CARTESIAN_POINT('Ctrl Pts',(7.12576974689923,1.37214155514399,-3.47578111318964));
#14816=CARTESIAN_POINT('Ctrl Pts',(7.07905715964822,1.43890221213298,-3.47156262682443));
#14817=CARTESIAN_POINT('Ctrl Pts',(7.02911865676118,1.50319561433792,-3.46734414045922));
#14818=CARTESIAN_POINT('Ctrl Pts',(6.97919652939898,1.56746793384827,-3.46312703739396));
#14819=CARTESIAN_POINT('Ctrl Pts',(6.92605087196958,1.62927423856367,-3.4589099343287));
#14820=CARTESIAN_POINT('Ctrl Pts',(6.86996117927447,1.68828261242724,-3.45469283126344));
#14821=CARTESIAN_POINT('Ctrl Pts',(6.81387271708422,1.74728969175544,-3.45047582071367));
#14822=CARTESIAN_POINT('Ctrl Pts',(6.75484066902482,1.80349862625898,-3.44625881016391));
#14823=CARTESIAN_POINT('Ctrl Pts',(6.69318229085379,1.8566134225701,-3.44204179961414));
#14824=CARTESIAN_POINT('Ctrl Pts',(6.63126888371411,1.90994791022124,-3.43780734683052));
#14825=CARTESIAN_POINT('Ctrl Pts',(6.56670772344626,1.96016229184336,-3.4335728940469));
#14826=CARTESIAN_POINT('Ctrl Pts',(6.49985311903929,2.00699806669602,-3.42933844126328));
#14827=CARTESIAN_POINT('Ctrl Pts',(6.43317736878537,2.0537085431804,-3.42511531678641));
#14828=CARTESIAN_POINT('Ctrl Pts',(6.36422084765703,2.09705825319777,-3.42089219230954));
#14829=CARTESIAN_POINT('Ctrl Pts',(6.29336207288622,2.13683556500231,-3.41666906783266));
#14830=CARTESIAN_POINT('Ctrl Pts',(6.22221818577473,2.17677292759111,-3.41242895089567));
#14831=CARTESIAN_POINT('Ctrl Pts',(6.14915713063745,2.21310888088526,-3.40818883395868));
#14832=CARTESIAN_POINT('Ctrl Pts',(6.07458301229684,2.2456776703852,-3.40394871702168));
#14833=CARTESIAN_POINT('Ctrl Pts',(6.00000889395624,2.27824645988515,-3.39970860008469));
#14834=CARTESIAN_POINT('Ctrl Pts',(5.92392217148605,2.30704797832714,-3.39546848314769));
#14835=CARTESIAN_POINT('Ctrl Pts',(5.84674123808758,2.33196711687165,-3.3912283662107));
#14836=CARTESIAN_POINT('Ctrl Pts',(5.7697064122947,2.35683908216358,-3.38699627604023));
#14837=CARTESIAN_POINT('Ctrl Pts',(5.69129412276694,2.37793615913287,-3.38276418586977));
#14838=CARTESIAN_POINT('Ctrl Pts',(5.61190875684904,2.39510786903117,-3.37853209569931));
#14839=CARTESIAN_POINT('Ctrl Pts',(5.53263685100436,2.41225503657913,-3.37430605416583));
#14840=CARTESIAN_POINT('Ctrl Pts',(5.45239508134243,2.42548788221613,-3.37008001263236));
#14841=CARTESIAN_POINT('Ctrl Pts',(5.37160391928243,2.43470538658716,-3.36585397109888));
#14842=CARTESIAN_POINT('Ctrl Pts',(5.29079054784242,2.44392542483754,-3.36162676783237));
#14843=CARTESIAN_POINT('Ctrl Pts',(5.20942793359722,2.44912779598835,-3.35739956456585));
#14844=CARTESIAN_POINT('Ctrl Pts',(5.12794809818051,2.45026243722329,-3.35317236129933));
#14845=CARTESIAN_POINT('Ctrl Pts',(5.04663641335074,2.45139473689005,-3.34895388174595));
#14846=CARTESIAN_POINT('Ctrl Pts',(4.96520845501238,2.44847604761854,-3.34473540219257));
#14847=CARTESIAN_POINT('Ctrl Pts',(4.88409785476334,2.44150852352233,-3.34051692263919));
#14848=CARTESIAN_POINT('Ctrl Pts',(4.80301385206782,2.43454328419647,-3.33629982639742));
#14849=CARTESIAN_POINT('Ctrl Pts',(4.72224746341948,2.42353188644212,-3.33208273015566));
#14850=CARTESIAN_POINT('Ctrl Pts',(4.64222921173274,2.40852850247356,-3.32786563391389));
#14851=CARTESIAN_POINT('Ctrl Pts',(4.56221271554549,2.39352544766032,-3.3236486301899));
#14852=CARTESIAN_POINT('Ctrl Pts',(4.48294478020379,2.37453066752952,-3.31943162646591));
#14853=CARTESIAN_POINT('Ctrl Pts',(4.40484630282877,2.35164955610249,-3.31521462274192));
#14854=CARTESIAN_POINT('Ctrl Pts',(4.32642452151457,2.32867372383447,-3.3109801619053));
#14855=CARTESIAN_POINT('Ctrl Pts',(4.24918235758169,2.30177943557109,-3.30674570106868));
#14856=CARTESIAN_POINT('Ctrl Pts',(4.17352938416566,2.27112356822859,-3.30251124023206));
#14857=CARTESIAN_POINT('Ctrl Pts',(4.09807906720647,2.24054982071795,-3.29828812251642));
#14858=CARTESIAN_POINT('Ctrl Pts',(4.02420984421193,2.20623485548807,-3.29406500480078));
#14859=CARTESIAN_POINT('Ctrl Pts',(3.95230510327355,2.16838134431833,-3.28984188708514));
#14860=CARTESIAN_POINT('Ctrl Pts',(3.88011066255758,2.13037532368087,-3.28560175468803));
#14861=CARTESIAN_POINT('Ctrl Pts',(3.80989696814085,2.08880243136719,-3.28136162229092));
#14862=CARTESIAN_POINT('Ctrl Pts',(3.74202281514706,2.04391175825419,-3.27712148989381));
#14863=CARTESIAN_POINT('Ctrl Pts',(3.67414866215327,1.99902108514119,-3.27288135749671));
#14864=CARTESIAN_POINT('Ctrl Pts',(3.60861439016784,1.95081295825972,-3.2686412250996));
#14865=CARTESIAN_POINT('Ctrl Pts',(3.54574405059633,1.89957599228275,-3.26440109270249));
#14866=CARTESIAN_POINT('Ctrl Pts',(3.48299299805349,1.84843624075493,-3.2601690053199));
#14867=CARTESIAN_POINT('Ctrl Pts',(3.42266165547484,1.79408835235942,-3.25593691793732));
#14868=CARTESIAN_POINT('Ctrl Pts',(3.36509614538569,1.73678995414854,-3.25170483055473));
#14869=CARTESIAN_POINT('Ctrl Pts',(3.30761291073701,1.67957344960877,-3.24747879187827));
#14870=CARTESIAN_POINT('Ctrl Pts',(3.25288798396186,1.61941513577923,-3.24325275320181));
#14871=CARTESIAN_POINT('Ctrl Pts',(3.20123471657503,1.55661302522545,-3.23902671452535));
#14872=CARTESIAN_POINT('Ctrl Pts',(3.14956720622137,1.49379359750235,-3.23479951055322));
#14873=CARTESIAN_POINT('Ctrl Pts',(3.10097339396209,1.42832922987503,-3.23057230658109));
#14874=CARTESIAN_POINT('Ctrl Pts',(3.05573013982453,1.36055532959373,-3.22634510260896));
#14875=CARTESIAN_POINT('Ctrl Pts',(3.01058029424646,1.29292135431376,-3.22212662606021));
#14876=CARTESIAN_POINT('Ctrl Pts',(2.96876746439428,1.2229877459403,-3.21790814951145));
#14877=CARTESIAN_POINT('Ctrl Pts',(2.93052555611176,1.15111964638223,-3.2136896729627));
#14878=CARTESIAN_POINT('Ctrl Pts',(2.89229618845911,1.07927511445655,-3.20947257977465));
#14879=CARTESIAN_POINT('Ctrl Pts',(2.85763563497825,1.00549776106932,-3.20525548658659));
#14880=CARTESIAN_POINT('Ctrl Pts',(2.82673244997499,0.930178394929204,-3.20103839339854));
#14881=CARTESIAN_POINT('Ctrl Pts',(2.79582994327943,0.854860682007235,-3.19682139277333));
#14882=CARTESIAN_POINT('Ctrl Pts',(2.76868481641195,0.778001453974088,-3.19260439214812));
#14883=CARTESIAN_POINT('Ctrl Pts',(2.74543739792786,0.700011283302266,-3.18838739152292));
#14884=CARTESIAN_POINT('Ctrl Pts',(2.72209370562171,0.621698134325635,-3.1841529271622));
#14885=CARTESIAN_POINT('Ctrl Pts',(2.70268022053618,0.542245104139516,-3.17991846280147));
#14886=CARTESIAN_POINT('Ctrl Pts',(2.68728790360722,0.462081247536648,-3.17568399844075));
#14887=CARTESIAN_POINT('Ctrl Pts',(2.67193684339092,0.382132257689247,-3.17146088390347));
#14888=CARTESIAN_POINT('Ctrl Pts',(2.66058544702283,0.301476715829103,-3.16723776936618));
#14889=CARTESIAN_POINT('Ctrl Pts',(2.65327200305062,0.220546589367562,-3.1630146548289));
#14890=CARTESIAN_POINT('Ctrl Pts',(2.64592907622978,0.139290207495064,-3.15877451555646));
#14891=CARTESIAN_POINT('Ctrl Pts',(2.6426567374437,0.0577574938856207,-3.15453437628402));
#14892=CARTESIAN_POINT('Ctrl Pts',(2.64344094462522,-0.0236149906744461,
-3.15029423701158));
#14893=CARTESIAN_POINT('Ctrl Pts',(2.64422515180675,-0.104987475234516,
-3.14605409773914));
#14894=CARTESIAN_POINT('Ctrl Pts',(2.64906581505127,-0.186199267937962,
-3.1418139584667));
#14895=CARTESIAN_POINT('Ctrl Pts',(2.65789683120988,-0.26682148607686,-3.13757381919427));
#14896=CARTESIAN_POINT('Ctrl Pts',(2.66671108470243,-0.347290670488414,
-3.13334172837711));
#14897=CARTESIAN_POINT('Ctrl Pts',(2.67953342467174,-0.427472732653372,
-3.12910963755995));
#14898=CARTESIAN_POINT('Ctrl Pts',(2.69633575485173,-0.506937110539796,
-3.12487754674279));
#14899=CARTESIAN_POINT('Ctrl Pts',(2.71311407055149,-0.586287915147322,
-3.12065150457842));
#14900=CARTESIAN_POINT('Ctrl Pts',(2.73386098347016,-0.664922621869127,
-3.11642546241405));
#14901=CARTESIAN_POINT('Ctrl Pts',(2.75849668580173,-0.742416222558389,
-3.11219942024968));
#14902=CARTESIAN_POINT('Ctrl Pts',(2.78313915584441,-0.819931111632119,
-3.10797221714286));
#14903=CARTESIAN_POINT('Ctrl Pts',(2.8116724750154,-0.896303807236035,-3.10374501403604));
#14904=CARTESIAN_POINT('Ctrl Pts',(2.8439656124048,-0.971119604946917,-3.09951781092922));
#14905=CARTESIAN_POINT('Ctrl Pts',(2.87619211189295,-1.04578101791411,-3.09529933078852));
#14906=CARTESIAN_POINT('Ctrl Pts',(2.91216276687888,-1.11889151541012,-3.09108085064782));
#14907=CARTESIAN_POINT('Ctrl Pts',(2.95169823903647,-1.19005628247225,-3.08686237050711));
#14908=CARTESIAN_POINT('Ctrl Pts',(2.99122074667082,-1.26119771309179,-3.08264527369588));
#14909=CARTESIAN_POINT('Ctrl Pts',(3.03430552449402,-1.33039427448151,-3.07842817688464));
#14910=CARTESIAN_POINT('Ctrl Pts',(3.08072703837876,-1.39727526587828,-3.07421108007341));
#14911=CARTESIAN_POINT('Ctrl Pts',(3.12714753362806,-1.46415478969372,-3.06999407579867));
#14912=CARTESIAN_POINT('Ctrl Pts',(3.17690435345151,-1.52871846345289,-3.06577707152393));
#14913=CARTESIAN_POINT('Ctrl Pts',(3.22972916030775,-1.59062532184517,-3.06156006724919));
#14914=CARTESIAN_POINT('Ctrl Pts',(3.28277263001954,-1.65278843731135,-3.05732560711893));
#14915=CARTESIAN_POINT('Ctrl Pts',(3.3389092436395,-1.7122723280798,-3.05309114698867));
#14916=CARTESIAN_POINT('Ctrl Pts',(3.39782831686894,-1.76876742098026,-3.04885668685841));
#14917=CARTESIAN_POINT('Ctrl Pts',(3.45658957655231,-1.82511119291694,-3.04463356864397));
#14918=CARTESIAN_POINT('Ctrl Pts',(3.5181180291659,-1.87848188213243,-3.04041045042953));
#14919=CARTESIAN_POINT('Ctrl Pts',(3.58207191229654,-1.92861254138529,-3.03618733221509));
#14920=CARTESIAN_POINT('Ctrl Pts',(3.64628343428149,-1.97894515249756,-3.03194720112691));
#14921=CARTESIAN_POINT('Ctrl Pts',(3.71293957967675,-2.02601130868253,-3.02770707003874));
#14922=CARTESIAN_POINT('Ctrl Pts',(3.78166628784708,-2.06958549171649,-3.02346693895057));
#14923=CARTESIAN_POINT('Ctrl Pts',(3.85039299601742,-2.11315967475046,-3.0192268078624));
#14924=CARTESIAN_POINT('Ctrl Pts',(3.92118982963898,-2.15324170852491,-3.01498667677422));
#14925=CARTESIAN_POINT('Ctrl Pts',(3.9936608735395,-2.18965394575042,-3.01074654568605));
#14926=CARTESIAN_POINT('Ctrl Pts',(4.06599447517755,-2.22599712670191,-3.00651445606076));
#14927=CARTESIAN_POINT('Ctrl Pts',(4.14026579677167,-2.25882002095934,-3.00228236643548));
#14928=CARTESIAN_POINT('Ctrl Pts',(4.21609817080659,-2.28791216603946,-2.99805027681019));
#14929=CARTESIAN_POINT('Ctrl Pts',(4.29182216231548,-2.31696273151442,-2.99382423584908));
#14930=CARTESIAN_POINT('Ctrl Pts',(4.36910234479523,-2.34229297294667,-2.98959819488797));
#14931=CARTESIAN_POINT('Ctrl Pts',(4.44753860300326,-2.36373885126346,-2.98537215392685));
#14932=CARTESIAN_POINT('Ctrl Pts',(4.52599643645029,-2.38519062863714,-2.98114495052065));
#14933=CARTESIAN_POINT('Ctrl Pts',(4.60561055332215,-2.40275572018323,-2.97691774711444));
#14934=CARTESIAN_POINT('Ctrl Pts',(4.6859616425133,-2.416318682077,-2.97269054370823));
#14935=CARTESIAN_POINT('Ctrl Pts',(4.76614689580707,-2.42985365149451,-2.96847206478948));
#14936=CARTESIAN_POINT('Ctrl Pts',(4.84706562832133,-2.43940289268036,-2.96425358587074));
#14937=CARTESIAN_POINT('Ctrl Pts',(4.92828896475836,-2.44490232062991,-2.96003510695199));
#14938=CARTESIAN_POINT('Ctrl Pts',(5.00948566624327,-2.45039994519379,-2.95581801136701));
#14939=CARTESIAN_POINT('Ctrl Pts',(5.09098631001662,-2.45185036249032,-2.95160091578203));
#14940=CARTESIAN_POINT('Ctrl Pts',(5.17235715004185,-2.44924137029201,-2.94738382019705));
#14941=CARTESIAN_POINT('Ctrl Pts',(5.25372620448142,-2.44663243534491,-2.94316681715119));
#14942=CARTESIAN_POINT('Ctrl Pts',(5.33496499642303,-2.43996428405567,-2.93894981410532));
#14943=CARTESIAN_POINT('Ctrl Pts',(5.41564147136897,-2.42927680515655,-2.93473281105946));
#14944=CARTESIAN_POINT('Ctrl Pts',(5.49665194950378,-2.41854507975266,-2.93049834948599));
#14945=CARTESIAN_POINT('Ctrl Pts',(5.57709497529563,-2.40376072474925,-2.92626388791252));
#14946=CARTESIAN_POINT('Ctrl Pts',(5.65654182376503,-2.38501623727525,-2.92202942633905));
#14947=CARTESIAN_POINT('Ctrl Pts',(5.73577582551224,-2.36632196831583,-2.91780630934732));
#14948=CARTESIAN_POINT('Ctrl Pts',(5.81401854313474,-2.34368892851612,-2.91358319235559));
#14949=CARTESIAN_POINT('Ctrl Pts',(5.89086013737419,-2.31725887110827,-2.90936007536386));
#14950=CARTESIAN_POINT('Ctrl Pts',(5.96801136159131,-2.29072231489381,-2.90511994149952));
#14951=CARTESIAN_POINT('Ctrl Pts',(6.04374971267005,-2.26035826006372,-2.90087980763518));
#14952=CARTESIAN_POINT('Ctrl Pts',(6.11768256730445,-2.22635809016041,-2.89663967377085));
#14953=CARTESIAN_POINT('Ctrl Pts',(6.19161542193886,-2.1923579202571,-2.89239953990651));
#14954=CARTESIAN_POINT('Ctrl Pts',(6.26374239458831,-2.15472190662379,-2.88815940604217));
#14955=CARTESIAN_POINT('Ctrl Pts',(6.33369916316487,-2.11368579843193,-2.88391927217784));
#14956=CARTESIAN_POINT('Ctrl Pts',(6.40352320772482,-2.0727275451384,-2.87968718281883));
#14957=CARTESIAN_POINT('Ctrl Pts',(6.47144578304493,-2.0282292937021,-2.87545509345982));
#14958=CARTESIAN_POINT('Ctrl Pts',(6.53708548680471,-1.9803927991649,-2.87122300410081));
#14959=CARTESIAN_POINT('Ctrl Pts',(6.60263137565911,-1.93262467447022,-2.86699696341417));
#14960=CARTESIAN_POINT('Ctrl Pts',(6.66590050076822,-1.88152805409757,-2.86277092272754));
#14961=CARTESIAN_POINT('Ctrl Pts',(6.7265376798801,-1.82734960897616,-2.8585448820409));
#14962=CARTESIAN_POINT('Ctrl Pts',(6.78719154319808,-1.7731562567572,-2.8543176785671));
#14963=CARTESIAN_POINT('Ctrl Pts',(6.84521162340756,-1.71587964237687,-2.8500904750933));
#14964=CARTESIAN_POINT('Ctrl Pts',(6.90027309242564,-1.65580896446282,-2.84586327161949));
#14965=CARTESIAN_POINT('Ctrl Pts',(6.95522091587987,-1.59586227100076,-2.84164479299322));
#14966=CARTESIAN_POINT('Ctrl Pts',(7.00722199651026,-1.53313336193388,-2.83742631436695));
#14967=CARTESIAN_POINT('Ctrl Pts',(7.05598941578056,-1.46794738125952,-2.83320783574069));
#14968=CARTESIAN_POINT('Ctrl Pts',(7.10474084304905,-1.40278277662549,-2.82899074045434));
#14969=CARTESIAN_POINT('Ctrl Pts',(7.15026043665294,-1.33516307229296,-2.82477364516799));
#14970=CARTESIAN_POINT('Ctrl Pts',(7.19230217857887,-1.2654457030301,-2.82055654988164));
#14971=CARTESIAN_POINT('Ctrl Pts',(7.23434299789154,-1.19572986372689,-2.81633954714017));
#14972=CARTESIAN_POINT('Ctrl Pts',(7.2729058782921,-1.12391684954804,-2.8121225443987));
#14973=CARTESIAN_POINT('Ctrl Pts',(7.30778944415839,-1.05039099110325,-2.80790554165724));
#14974=CARTESIAN_POINT('Ctrl Pts',(7.34281743446293,-0.97656072195563,-2.8036710797416));
#14975=CARTESIAN_POINT('Ctrl Pts',(7.37413536537025,-0.9010038160837,-2.79943661782597));
#14976=CARTESIAN_POINT('Ctrl Pts',(7.40158782827053,-0.824130406548198,
-2.79520215591033));
#14977=CARTESIAN_POINT('Ctrl Pts',(7.42896673878781,-0.747462961136234,
-2.79097903923413));
#14978=CARTESIAN_POINT('Ctrl Pts',(7.45250077237866,-0.669486517101287,
-2.78675592255792));
#14979=CARTESIAN_POINT('Ctrl Pts',(7.47208612987216,-0.590622130126553,
-2.78253280588172));
#14980=CARTESIAN_POINT('Ctrl Pts',(7.49175041032252,-0.511439943968847,
-2.77829267134637));
#14981=CARTESIAN_POINT('Ctrl Pts',(7.50743404143823,-0.431363107805052,
-2.77405253681102));
#14982=CARTESIAN_POINT('Ctrl Pts',(7.51908423982023,-0.350825205375978,
-2.76981240227567));
#14983=CARTESIAN_POINT('Ctrl Pts',(7.53073443820223,-0.270287302946905,
-2.76557226774032));
#14984=CARTESIAN_POINT('Ctrl Pts',(7.53835122203186,-0.189288805356301,
-2.76133213320497));
#14985=CARTESIAN_POINT('Ctrl Pts',(7.5419344305525,-0.10826365782412,-2.75709199866962));
#14986=CARTESIAN_POINT('Ctrl Pts',(7.54351950878196,-0.072421144988782,
-2.75521632079508));
#14987=CARTESIAN_POINT('Ctrl Pts',(7.54431748352352,-0.0365435678230778,
-2.75334064292055));
#14988=CARTESIAN_POINT('Ctrl Pts',(7.54432706806718,-0.000654429855887372,
-2.75146496504602));
#14989=CARTESIAN_POINT('',(7.54432654498802,-0.00172970779088622,-1.95146499540829));
#14990=CARTESIAN_POINT('Ctrl Pts',(7.54432706806737,-0.000654429150524658,
-2.75146496500915));
#14991=CARTESIAN_POINT('Ctrl Pts',(7.54434854189861,0.0797540024314393,
-2.74726257050805));
#14992=CARTESIAN_POINT('Ctrl Pts',(7.54040807903265,0.160320975657735,-2.74306017600695));
#14993=CARTESIAN_POINT('Ctrl Pts',(7.53248499309161,0.24062044992958,-2.73885778150585));
#14994=CARTESIAN_POINT('Ctrl Pts',(7.5245730202728,0.320807294112681,-2.73466128139036));
#14995=CARTESIAN_POINT('Ctrl Pts',(7.51268956108371,0.400726918697619,-2.73046478127487));
#14996=CARTESIAN_POINT('Ctrl Pts',(7.49686594348856,0.479952948940973,-2.72626828115938));
#14997=CARTESIAN_POINT('Ctrl Pts',(7.48105969025352,0.559092038931199,-2.72207638615639));
#14998=CARTESIAN_POINT('Ctrl Pts',(7.46132196055022,0.637538586300265,-2.7178844911534));
#14999=CARTESIAN_POINT('Ctrl Pts',(7.43773574774814,0.714872548756429,-2.71369259615041));
#15000=CARTESIAN_POINT('Ctrl Pts',(7.41416339531342,0.792161066141067,-2.70950316450196));
#15001=CARTESIAN_POINT('Ctrl Pts',(7.38674718490084,0.868337845776393,-2.70531373285352));
#15002=CARTESIAN_POINT('Ctrl Pts',(7.35562063744385,0.942995490351987,-2.70112430120508));
#15003=CARTESIAN_POINT('Ctrl Pts',(7.32450251971678,1.01763291605235,-2.69693600414368));
#15004=CARTESIAN_POINT('Ctrl Pts',(7.28967624164218,1.09075158831796,-2.69274770708227));
#15005=CARTESIAN_POINT('Ctrl Pts',(7.25132384901173,1.16196310926106,-2.68855941002087));
#15006=CARTESIAN_POINT('Ctrl Pts',(7.21296969206233,1.23317790613631,-2.68437092028591));
#15007=CARTESIAN_POINT('Ctrl Pts',(7.1710893240234,1.30248496302861,-2.68018243055095));
#15008=CARTESIAN_POINT('Ctrl Pts',(7.12591049593355,1.36952091891357,-2.67599394081599));
#15009=CARTESIAN_POINT('Ctrl Pts',(7.08068583935419,1.43662487471642,-2.67180120236175));
#15010=CARTESIAN_POINT('Ctrl Pts',(7.03215630756797,1.50145273850618,-2.66760846390752));
#15011=CARTESIAN_POINT('Ctrl Pts',(6.98059231043497,1.56367116106497,-2.66341572545328));
#15012=CARTESIAN_POINT('Ctrl Pts',(6.92900025385767,1.62592344085863,-2.65922070544762));
#15013=CARTESIAN_POINT('Ctrl Pts',(6.87437076450931,1.68556310558168,-2.65502568544195));
#15014=CARTESIAN_POINT('Ctrl Pts',(6.81701204744791,1.74229276472149,-2.65083066543629));
#15015=CARTESIAN_POINT('Ctrl Pts',(6.75955608568052,1.79911860207635,-2.64662853328608));
#15016=CARTESIAN_POINT('Ctrl Pts',(6.69936201011216,1.85302426976348,-2.64242640113586));
#15017=CARTESIAN_POINT('Ctrl Pts',(6.63677172151105,1.90375216771309,-2.63822426898564));
#15018=CARTESIAN_POINT('Ctrl Pts',(6.59725288303542,1.93578121966481,-2.6355710877109));
#15019=CARTESIAN_POINT('Ctrl Pts',(6.5567794139668,1.96654429048435,-2.63291790643615));
#15020=CARTESIAN_POINT('Ctrl Pts',(6.51544287596956,1.99598571968351,-2.6302647251614));
#15021=CARTESIAN_POINT('Ctrl Pts',(6.44950696129238,2.04294774547725,-2.62603263552277));
#15022=CARTESIAN_POINT('Ctrl Pts',(6.38111851702674,2.08672664771273,-2.62180054588414));
#15023=CARTESIAN_POINT('Ctrl Pts',(6.31061765686899,2.12705691641387,-2.61756845624552));
#15024=CARTESIAN_POINT('Ctrl Pts',(6.2402175592768,2.16732954352972,-2.61334241527365));
#15025=CARTESIAN_POINT('Ctrl Pts',(6.16771144212945,2.20416309767123,-2.60911637430179));
#15026=CARTESIAN_POINT('Ctrl Pts',(6.09346968054336,2.23733436750772,-2.60489033332993));
#15027=CARTESIAN_POINT('Ctrl Pts',(6.01920749772839,2.27051476156325,-2.60066312992673));
#15028=CARTESIAN_POINT('Ctrl Pts',(5.94320911055678,2.30003060757775,-2.59643592652353));
#15029=CARTESIAN_POINT('Ctrl Pts',(5.86587128518856,2.32570378847802,-2.59220872312033));
#15030=CARTESIAN_POINT('Ctrl Pts',(5.78869307653494,2.3513239827735,-2.58799024419725));
#15031=CARTESIAN_POINT('Ctrl Pts',(5.7101813862433,2.37311718764522,-2.58377176527416));
#15032=CARTESIAN_POINT('Ctrl Pts',(5.63075027478648,2.39095458215444,-2.57955328635107));
#15033=CARTESIAN_POINT('Ctrl Pts',(5.55134521061696,2.40878612737198,-2.57533619076419));
#15034=CARTESIAN_POINT('Ctrl Pts',(5.4710217770792,2.42266433661221,-2.57111909517731));
#15035=CARTESIAN_POINT('Ctrl Pts',(5.39020677054793,2.4325109195554,-2.56690199959043));
#15036=CARTESIAN_POINT('Ctrl Pts',(5.30939353745222,2.44235728642139,-2.56268499654511));
#15037=CARTESIAN_POINT('Ctrl Pts',(5.22808921422736,2.44817214783349,-2.5584679934998));
#15038=CARTESIAN_POINT('Ctrl Pts',(5.1467268796151,2.44992895186444,-2.55425099045448));
#15039=CARTESIAN_POINT('Ctrl Pts',(5.0650277024515,2.45169302911775,-2.55001652888771));
#15040=CARTESIAN_POINT('Ctrl Pts',(4.98327050395485,2.44936535339045,-2.54578206732093));
#15041=CARTESIAN_POINT('Ctrl Pts',(4.90189310547216,2.4429718726293,-2.54154760575416));
#15042=CARTESIAN_POINT('Ctrl Pts',(4.8207337258634,2.43659552069632,-2.53732448876905));
#15043=CARTESIAN_POINT('Ctrl Pts',(4.73995257228229,2.42617522202766,-2.53310137178393));
#15044=CARTESIAN_POINT('Ctrl Pts',(4.65997632302281,2.41178848682871,-2.52887825479882));
#15045=CARTESIAN_POINT('Ctrl Pts',(4.57967781282647,2.39734378088462,-2.52463812094121));
#15046=CARTESIAN_POINT('Ctrl Pts',(4.50019116460046,2.37890072070823,-2.52039798708361));
#15047=CARTESIAN_POINT('Ctrl Pts',(4.4219336209134,2.35658849361609,-2.516157853226));
#15048=CARTESIAN_POINT('Ctrl Pts',(4.34367607722634,2.33427626652394,-2.5119177193684));
#15049=CARTESIAN_POINT('Ctrl Pts',(4.2666480605307,2.30809508180683,-2.50767758551079));
#15050=CARTESIAN_POINT('Ctrl Pts',(4.19124561850368,2.27822229362238,-2.50343745165319));
#15051=CARTESIAN_POINT('Ctrl Pts',(4.11598622740783,2.2484061790688,-2.49920536203235));
#15052=CARTESIAN_POINT('Ctrl Pts',(4.04206546527402,2.21480123235921,-2.49497327241151));
#15053=CARTESIAN_POINT('Ctrl Pts',(3.96989106897527,2.17754860416774,-2.49074118279068));
#15054=CARTESIAN_POINT('Ctrl Pts',(3.89781982714067,2.14034921888645,-2.48651514183751));
#15055=CARTESIAN_POINT('Ctrl Pts',(3.82749040334373,2.09951271787029,-2.48228910088433));
#15056=CARTESIAN_POINT('Ctrl Pts',(3.75929148032207,2.05522864465308,-2.47806305993116));
#15057=CARTESIAN_POINT('Ctrl Pts',(3.69107379786298,2.01093239024204,-2.4738358565234));
#15058=CARTESIAN_POINT('Ctrl Pts',(3.62498821192454,1.96318686309778,-2.46960865311564));
#15059=CARTESIAN_POINT('Ctrl Pts',(3.56139990073682,1.91222827063159,-2.46538144970789));
#15060=CARTESIAN_POINT('Ctrl Pts',(3.49794282916828,1.86137485136696,-2.46116297080555));
#15061=CARTESIAN_POINT('Ctrl Pts',(3.43697311269183,1.80732188750033,-2.45694449190321));
#15062=CARTESIAN_POINT('Ctrl Pts',(3.37882395333543,1.75034689896777,-2.45272601300086));
#15063=CARTESIAN_POINT('Ctrl Pts',(3.32069386243527,1.69339059385365,-2.44850891743547));
#15064=CARTESIAN_POINT('Ctrl Pts',(3.26538282349842,1.63351449193571,-2.44429182187007));
#15065=CARTESIAN_POINT('Ctrl Pts',(3.21318854831966,1.5710342705871,-2.44007472630467));
#15066=CARTESIAN_POINT('Ctrl Pts',(3.16099541852096,1.50855542033906,-2.43585772328155));
#15067=CARTESIAN_POINT('Ctrl Pts',(3.11191921352454,1.44347292164478,-2.43164072025844));
#15068=CARTESIAN_POINT('Ctrl Pts',(3.06621763312194,1.37613584901781,-2.42742371723532));
#15069=CARTESIAN_POINT('Ctrl Pts',(3.02032684627744,1.30851999811211,-2.42318925564445));
#15070=CARTESIAN_POINT('Ctrl Pts',(2.97783896132905,1.23863124859839,-2.41895479405359));
#15071=CARTESIAN_POINT('Ctrl Pts',(2.93897018993233,1.16685119366035,-2.41472033246273));
#15072=CARTESIAN_POINT('Ctrl Pts',(2.9002055526267,1.09526344608142,-2.41049721550133));
#15073=CARTESIAN_POINT('Ctrl Pts',(2.86504082628886,1.02179495373373,-2.40627409853992));
#15074=CARTESIAN_POINT('Ctrl Pts',(2.83364288628048,0.946845985039064,-2.40205098157852));
#15075=CARTESIAN_POINT('Ctrl Pts',(2.80211842905802,0.871595011349318,-2.39781084767292));
#15076=CARTESIAN_POINT('Ctrl Pts',(2.77439133068076,0.794852051365718,-2.39357071376733));
#15077=CARTESIAN_POINT('Ctrl Pts',(2.75057996189763,0.717037544271118,-2.38933057986174));
#15078=CARTESIAN_POINT('Ctrl Pts',(2.7267685931145,0.639223037176518,-2.38509044595615));
#15079=CARTESIAN_POINT('Ctrl Pts',(2.70687300789286,0.560337451325784,-2.38085031205056));
#15080=CARTESIAN_POINT('Ctrl Pts',(2.69095962667335,0.480809618389507,-2.37661017814497));
#15081=CARTESIAN_POINT('Ctrl Pts',(2.67507643570977,0.401432662604738,-2.37237808845864));
#15082=CARTESIAN_POINT('Ctrl Pts',(2.6631010802132,0.321119758273199,-2.36814599877231));
#15083=CARTESIAN_POINT('Ctrl Pts',(2.65513672227431,0.240289868954506,-2.36391390908598));
#15084=CARTESIAN_POINT('Ctrl Pts',(2.64718374730434,0.159575504845203,-2.3596878680662));
#15085=CARTESIAN_POINT('Ctrl Pts',(2.64323042936626,0.0783460818593184,
-2.35546182704641));
#15086=CARTESIAN_POINT('Ctrl Pts',(2.64332895420887,-0.00296912424105906,
-2.35123578602663));
#15087=CARTESIAN_POINT('Ctrl Pts',(2.64342750615072,-0.0843066960672667,
-2.34700858263538));
#15088=CARTESIAN_POINT('Ctrl Pts',(2.64758019548345,-0.165729635981154,
-2.34278137924414));
#15089=CARTESIAN_POINT('Ctrl Pts',(2.65578726371151,-0.24680303133594,-2.33855417585289));
#15090=CARTESIAN_POINT('Ctrl Pts',(2.66397739357534,-0.327709101324162,
-2.33433569688171));
#15091=CARTESIAN_POINT('Ctrl Pts',(2.67620516165348,-0.408266603271003,
-2.33011721791053));
#15092=CARTESIAN_POINT('Ctrl Pts',(2.69241875185148,-0.488045007260048,
-2.32589873893934));
#15093=CARTESIAN_POINT('Ctrl Pts',(2.70862702524044,-0.567797250076017,
-2.32168164330441));
#15094=CARTESIAN_POINT('Ctrl Pts',(2.72881843260493,-0.646770447274864,
-2.31746454766949));
#15095=CARTESIAN_POINT('Ctrl Pts',(2.75288983833641,-0.7245431162674,-2.31324745203456));
#15096=CARTESIAN_POINT('Ctrl Pts',(2.77696071583506,-0.802314078584467,
-2.30903044894131));
#15097=CARTESIAN_POINT('Ctrl Pts',(2.80491128391827,-0.878884121503322,
-2.30481344584807));
#15098=CARTESIAN_POINT('Ctrl Pts',(2.83658862510449,-0.953847192746091,
-2.30059644275482));
#15099=CARTESIAN_POINT('Ctrl Pts',(2.86839711066191,-1.02912061152666,-2.29636198124498));
#15100=CARTESIAN_POINT('Ctrl Pts',(2.90396312099272,-1.10277328493736,-2.29212751973514));
#15101=CARTESIAN_POINT('Ctrl Pts',(2.94308389171767,-1.17441630757438,-2.2878930582253));
#15102=CARTESIAN_POINT('Ctrl Pts',(2.98209985461661,-1.24586739254472,-2.28366994119301));
#15103=CARTESIAN_POINT('Ctrl Pts',(3.02465127585166,-1.31531920385023,-2.27944682416072));
#15104=CARTESIAN_POINT('Ctrl Pts',(3.0704928975755,-1.38241409530533,-2.27522370712843));
#15105=CARTESIAN_POINT('Ctrl Pts',(3.11651923449117,-1.44977934032297,-2.27098357337982));
#15106=CARTESIAN_POINT('Ctrl Pts',(3.16586205112207,-1.51476826107824,-2.26674343963121));
#15107=CARTESIAN_POINT('Ctrl Pts',(3.21823279302944,-1.57705295968289,-2.26250330588259));
#15108=CARTESIAN_POINT('Ctrl Pts',(3.27060353493681,-1.63933765828753,-2.25826317213398));
#15109=CARTESIAN_POINT('Ctrl Pts',(3.32600183833949,-1.69891783485511,-2.25402303838536));
#15110=CARTESIAN_POINT('Ctrl Pts',(3.38410386532837,-1.75550463434451,-2.24978290463675));
#15111=CARTESIAN_POINT('Ctrl Pts',(3.44209566508421,-1.81198408118791,-2.2455508149829));
#15112=CARTESIAN_POINT('Ctrl Pts',(3.50299728362785,-1.86569222295865,-2.24131872532904));
#15113=CARTESIAN_POINT('Ctrl Pts',(3.5665131379305,-1.91631472933831,-2.23708663567519));
#15114=CARTESIAN_POINT('Ctrl Pts',(3.62993821290689,-1.9668648840654,-2.23286059468827));
#15115=CARTESIAN_POINT('Ctrl Pts',(3.69596974245664,-2.01433787515399,-2.22863455370135));
#15116=CARTESIAN_POINT('Ctrl Pts',(3.76427577817638,-2.05845655411562,-2.22440851271442));
#15117=CARTESIAN_POINT('Ctrl Pts',(3.83260060211639,-2.1025873683366,-2.22018130931501));
#15118=CARTESIAN_POINT('Ctrl Pts',(3.9032008312208,-2.14336171876791,-2.2159541059156));
#15119=CARTESIAN_POINT('Ctrl Pts',(3.97571154982797,-2.18054299257261,-2.21172690251619));
#15120=CARTESIAN_POINT('Ctrl Pts',(4.04807261464879,-2.21764752850307,-2.20750842357857));
#15121=CARTESIAN_POINT('Ctrl Pts',(4.12233588867037,-2.25117357010027,-2.20328994464096));
#15122=CARTESIAN_POINT('Ctrl Pts',(4.19811183741015,-2.28093058180717,-2.19907146570334));
#15123=CARTESIAN_POINT('Ctrl Pts',(4.27386293747027,-2.31067783550425,-2.19485437010218));
#15124=CARTESIAN_POINT('Ctrl Pts',(4.35112529495758,-2.33665834407526,-2.19063727450101));
#15125=CARTESIAN_POINT('Ctrl Pts',(4.42948907302834,-2.35872956530421,-2.18642017889984));
#15126=CARTESIAN_POINT('Ctrl Pts',(4.50785113144961,-2.38080030219249,-2.18220317584049));
#15127=CARTESIAN_POINT('Ctrl Pts',(4.58731411480005,-2.3989617974339,-2.17798617278114));
#15128=CARTESIAN_POINT('Ctrl Pts',(4.66745407730865,-2.4131216811909,-2.17376916972179));
#15129=CARTESIAN_POINT('Ctrl Pts',(4.74792582111344,-2.42734018719379,-2.16953470817235));
#15130=CARTESIAN_POINT('Ctrl Pts',(4.82907969906962,-2.43752378283115,-2.16530024662292));
#15131=CARTESIAN_POINT('Ctrl Pts',(4.91047906191892,-2.44363125831157,-2.16106578507348));
#15132=CARTESIAN_POINT('Ctrl Pts',(4.9916603476364,-2.44972237124701,-2.15684266807512));
#15133=CARTESIAN_POINT('Ctrl Pts',(5.07308533611021,-2.45175920627896,-2.15261955107676));
#15134=CARTESIAN_POINT('Ctrl Pts',(5.15432051711643,-2.44975321271239,-2.1483964340784));
#15135=CARTESIAN_POINT('Ctrl Pts',(5.2358830309886,-2.44773913610082,-2.14415630025342));
#15136=CARTESIAN_POINT('Ctrl Pts',(5.31725373503625,-2.44164962516456,-2.13991616642844));
#15137=CARTESIAN_POINT('Ctrl Pts',(5.39800055324951,-2.43154864110776,-2.13567603260347));
#15138=CARTESIAN_POINT('Ctrl Pts',(5.47874737146277,-2.42144765705095,-2.13143589877849));
#15139=CARTESIAN_POINT('Ctrl Pts',(5.55886985438538,-2.40733534220338,-2.12719576495352));
#15140=CARTESIAN_POINT('Ctrl Pts',(5.6379495174793,-2.38932649613715,-2.12295563112854));
#15141=CARTESIAN_POINT('Ctrl Pts',(5.71687915457629,-2.37135181555644,-2.1187235414742));
#15142=CARTESIAN_POINT('Ctrl Pts',(5.79506439894685,-2.34942833051731,-2.11449145181987));
#15143=CARTESIAN_POINT('Ctrl Pts',(5.8720807420363,-2.32363327678238,-2.11025936216553));
#15144=CARTESIAN_POINT('Ctrl Pts',(5.94898701037529,-2.29787509034065,-2.1060333211782));
#15145=CARTESIAN_POINT('Ctrl Pts',(6.02472725855494,-2.26825647147638,-2.10180728019086));
#15146=CARTESIAN_POINT('Ctrl Pts',(6.09888841933066,-2.23490539080581,-2.09758123920352));
#15147=CARTESIAN_POINT('Ctrl Pts',(6.17306997882485,-2.20154513660966,-2.09335403580422));
#15148=CARTESIAN_POINT('Ctrl Pts',(6.24567113357853,-2.16445049642864,-2.08912683240492));
#15149=CARTESIAN_POINT('Ctrl Pts',(6.31629491986107,-2.12379914657281,-2.08489962900562));
#15150=CARTESIAN_POINT('Ctrl Pts',(6.38677294677355,-2.0832316964264,-2.08068115006782));
#15151=CARTESIAN_POINT('Ctrl Pts',(6.45528134395092,-2.03912241338662,-2.07646267113002));
#15152=CARTESIAN_POINT('Ctrl Pts',(6.52144844062969,-1.99169468446114,-2.07224419219222));
#15153=CARTESIAN_POINT('Ctrl Pts',(6.58759383959166,-1.94428250818165,-2.06802709659095));
#15154=CARTESIAN_POINT('Ctrl Pts',(6.65139908537569,-1.89355431758331,-2.06381000098967));
#15155=CARTESIAN_POINT('Ctrl Pts',(6.712521754789,-1.83977662885493,-2.05959290538839));
#15156=CARTESIAN_POINT('Ctrl Pts',(6.77364308289814,-1.78600012024906,-2.05537590232902));
#15157=CARTESIAN_POINT('Ctrl Pts',(6.8320816035631,-1.72917455438314,-2.05115889926964));
#15158=CARTESIAN_POINT('Ctrl Pts',(6.88752933678303,-1.66960556260821,-2.04694189621026));
#15159=CARTESIAN_POINT('Ctrl Pts',(6.94320662489548,-1.60978995383543,-2.0427074346611));
#15160=CARTESIAN_POINT('Ctrl Pts',(6.9958679780722,-1.54720849164571,-2.03847297311194));
#15161=CARTESIAN_POINT('Ctrl Pts',(7.04524145247997,-1.48220527976363,-2.03423851156278));
#15162=CARTESIAN_POINT('Ctrl Pts',(7.09448265035379,-1.41737621806373,-2.03001539456458));
#15163=CARTESIAN_POINT('Ctrl Pts',(7.1404533341697,-1.35013877554761,-2.02579227756639));
#15164=CARTESIAN_POINT('Ctrl Pts',(7.18292746618936,-1.28086304563826,-2.02156916056819));
#15165=CARTESIAN_POINT('Ctrl Pts',(7.2255727454762,-1.2113081728414,-2.01732902674354));
#15166=CARTESIAN_POINT('Ctrl Pts',(7.2646930166829,-1.13969896950011,-2.0130888929189));
#15167=CARTESIAN_POINT('Ctrl Pts',(7.30010709790759,-1.0664328696749,-2.00884875909425));
#15168=CARTESIAN_POINT('Ctrl Pts',(7.33552117913229,-0.993166769849684,
-2.00460862526961));
#15169=CARTESIAN_POINT('Ctrl Pts',(7.3672289455247,-0.918244228162472,-2.00036849144496));
#15170=CARTESIAN_POINT('Ctrl Pts',(7.39509927478015,-0.842078905333729,
-1.99612835762031));
#15171=CARTESIAN_POINT('Ctrl Pts',(7.42717646114053,-0.754416889137817,
-1.99124820132078));
#15172=CARTESIAN_POINT('Ctrl Pts',(7.45427036000956,-0.664839421422339,
-1.98636804502124));
#15173=CARTESIAN_POINT('Ctrl Pts',(7.47618097156536,-0.573881995583924,
-1.9814878887217));
#15174=CARTESIAN_POINT('Ctrl Pts',(7.49864678047242,-0.480619781411635,
-1.97648407316947));
#15175=CARTESIAN_POINT('Ctrl Pts',(7.51566290806625,-0.385906846851153,
-1.97148025761723));
#15176=CARTESIAN_POINT('Ctrl Pts',(7.52706584652748,-0.290344144522799,
-1.96647644206499));
#15177=CARTESIAN_POINT('Ctrl Pts',(7.53846878498872,-0.194781442194444,
-1.96147262651276));
#15178=CARTESIAN_POINT('Ctrl Pts',(7.54425833113807,-0.0983691509038746,
-1.95646881096052));
#15179=CARTESIAN_POINT('Ctrl Pts',(7.54432654498802,-0.00172970779088622,
-1.95146499540829));
#15180=CARTESIAN_POINT('',(7.54193252997112,0.00182552697798459,-1.15146496504602));
#15181=CARTESIAN_POINT('Ctrl Pts',(7.54171139332785,-0.00172727609620038,
-1.95146496504602));
#15182=CARTESIAN_POINT('Ctrl Pts',(7.53826048626319,0.526658739318973,-1.92407700473471));
#15183=CARTESIAN_POINT('Ctrl Pts',(7.11114846716908,1.87574080279579,-1.85441328658734));
#15184=CARTESIAN_POINT('Ctrl Pts',(4.88956789803041,2.88771064714606,-1.74247381060388));
#15185=CARTESIAN_POINT('Ctrl Pts',(2.55897587967682,1.39825735648593,-1.61564653709567));
#15186=CARTESIAN_POINT('Ctrl Pts',(2.54229394979133,-1.3675792209613,-1.48881926358746));
#15187=CARTESIAN_POINT('Ctrl Pts',(4.8547500177879,-2.88503669780044,-1.36199199007923));
#15188=CARTESIAN_POINT('Ctrl Pts',(7.09859127194373,-1.89543272355351,-1.24954055723209));
#15189=CARTESIAN_POINT('Ctrl Pts',(7.53819513999477,-0.536315133329038,
-1.17936488222102));
#15190=CARTESIAN_POINT('Ctrl Pts',(7.54193252997112,0.00182552697798459,
-1.15146496504602));
#15191=CARTESIAN_POINT('',(7.54820283579053,0.000480549568469427,-0.351464965046016));
#15192=CARTESIAN_POINT('Ctrl Pts',(7.54193252997112,0.00182552697798459,
-1.15146496504602));
#15193=CARTESIAN_POINT('Ctrl Pts',(7.54385827485599,0.279110378301824,-1.13708912438495));
#15194=CARTESIAN_POINT('Ctrl Pts',(7.3724979850303,1.36951155024719,-1.08043752588781));
#15195=CARTESIAN_POINT('Ctrl Pts',(5.77063349163689,2.81469852890825,-0.981510169554581));
#15196=CARTESIAN_POINT('Ctrl Pts',(3.09918935794445,2.09809787237654,-0.854682896046374));
#15197=CARTESIAN_POINT('Ctrl Pts',(2.24852759774879,-0.533727507488469,
-0.727855622538154));
#15198=CARTESIAN_POINT('Ctrl Pts',(3.99516510083363,-2.67834581692979,-0.601028349029938));
#15199=CARTESIAN_POINT('Ctrl Pts',(6.715139087859,-2.3812954588471,-0.475564796532559));
#15200=CARTESIAN_POINT('Ctrl Pts',(7.54609087854429,-0.78345086191955,-0.39237700187125));
#15201=CARTESIAN_POINT('Ctrl Pts',(7.54820283579053,0.000480549568469427,
-0.351464965046016));
#15202=CARTESIAN_POINT('',(7.54432619069004,-0.00217446611864238,0.448535034953988));
#15203=CARTESIAN_POINT('Ctrl Pts',(7.54820283579053,0.000480549568469427,
-0.351464965046016));
#15204=CARTESIAN_POINT('Ctrl Pts',(7.54827323366592,0.0266113369811877,
-0.350101244035178));
#15205=CARTESIAN_POINT('Ctrl Pts',(7.53607092417593,0.862736984340334,-0.306461765188222));
#15206=CARTESIAN_POINT('Ctrl Pts',(6.58857745365878,2.47917651072543,-0.220546528505332));
#15207=CARTESIAN_POINT('Ctrl Pts',(3.82543063400702,2.60226149525943,-0.0937192549970498));
#15208=CARTESIAN_POINT('Ctrl Pts',(2.22012511854379,0.349901741046586,0.0331080185111337));
#15209=CARTESIAN_POINT('Ctrl Pts',(3.23804574570049,-2.22186182840879,0.159935292019368));
#15210=CARTESIAN_POINT('Ctrl Pts',(5.94999527582803,-2.76542415824012,0.286762565527575));
#15211=CARTESIAN_POINT('Ctrl Pts',(7.41422764622619,-1.26294971488547,0.382962317259512));
#15212=CARTESIAN_POINT('Ctrl Pts',(7.54523656020964,-0.22653931857562,0.436886311155375));
#15213=CARTESIAN_POINT('Ctrl Pts',(7.54330296331732,-0.00218295240421028,
0.448534547215166));
#15214=CARTESIAN_POINT('',(7.54432692296551,0.00106743696237302,1.24853503500156));
#15215=CARTESIAN_POINT('Ctrl Pts',(7.54432619069003,-0.00217446611864238,
0.448535034953988));
#15216=CARTESIAN_POINT('Ctrl Pts',(7.54439769743544,0.0784095490257859,
0.452717120495905));
#15217=CARTESIAN_POINT('Ctrl Pts',(7.54048996103696,0.159079511651245,0.456899206037822));
#15218=CARTESIAN_POINT('Ctrl Pts',(7.53260427432528,0.23940846782338,0.461081291579739));
#15219=CARTESIAN_POINT('Ctrl Pts',(7.52472246292544,0.319697947439349,0.465261321893471));
#15220=CARTESIAN_POINT('Ctrl Pts',(7.51286662670644,0.399646282378622,0.469441352207201));
#15221=CARTESIAN_POINT('Ctrl Pts',(7.4970900754961,0.478829392525623,0.473621382520934));
#15222=CARTESIAN_POINT('Ctrl Pts',(7.48131623537897,0.557998895592729,0.477800694524835));
#15223=CARTESIAN_POINT('Ctrl Pts',(7.46162311120078,0.636402970472835,0.481980006528739));
#15224=CARTESIAN_POINT('Ctrl Pts',(7.43811525099534,0.713627056030673,0.48615931853264));
#15225=CARTESIAN_POINT('Ctrl Pts',(7.41460391741901,0.790862551724844,0.490339248044919));
#15226=CARTESIAN_POINT('Ctrl Pts',(7.38727686924614,0.866917259459341,0.494519177557197));
#15227=CARTESIAN_POINT('Ctrl Pts',(7.35628824494104,0.941392621892211,0.498699107069475));
#15228=CARTESIAN_POINT('Ctrl Pts',(7.32526596372127,1.01594887242432,0.502883576426102));
#15229=CARTESIAN_POINT('Ctrl Pts',(7.29057435498377,1.08892191757199,0.507068045782728));
#15230=CARTESIAN_POINT('Ctrl Pts',(7.25241504782299,1.15993472269526,0.511252515139354));
#15231=CARTESIAN_POINT('Ctrl Pts',(7.21423132633598,1.23099296181407,0.515439661719641));
#15232=CARTESIAN_POINT('Ctrl Pts',(7.17257573845089,1.30008806150189,0.519626808299931));
#15233=CARTESIAN_POINT('Ctrl Pts',(7.12769372869992,1.36687124932426,0.523813954880218));
#15234=CARTESIAN_POINT('Ctrl Pts',(7.08273896064374,1.43376269949027,0.528007889251217));
#15235=CARTESIAN_POINT('Ctrl Pts',(7.03454762087561,1.49833438387621,0.532201823622214));
#15236=CARTESIAN_POINT('Ctrl Pts',(6.98340547657611,1.56027049524818,0.536395757993212));
#15237=CARTESIAN_POINT('Ctrl Pts',(6.96705959253474,1.58006631156223,0.537736209510145));
#15238=CARTESIAN_POINT('Ctrl Pts',(6.95041254789911,1.599593177255,0.539076661027078));
#15239=CARTESIAN_POINT('Ctrl Pts',(6.9334744274315,1.61884161198756,0.54041711254401));
#15240=CARTESIAN_POINT('Ctrl Pts',(6.8799971896741,1.67961300174232,0.544649202202974));
#15241=CARTESIAN_POINT('Ctrl Pts',(6.82340565434219,1.73784503569686,0.548881291861938));
#15242=CARTESIAN_POINT('Ctrl Pts',(6.76397035957675,1.79320158591264,0.553113381520903));
#15243=CARTESIAN_POINT('Ctrl Pts',(6.70462001204309,1.84847901839677,0.557339422512949));
#15244=CARTESIAN_POINT('Ctrl Pts',(6.64243431464192,1.90088881549488,0.561565463504997));
#15245=CARTESIAN_POINT('Ctrl Pts',(6.57772292224304,1.95012912477685,0.565791504497043));
#15246=CARTESIAN_POINT('Ctrl Pts',(6.51299373046252,1.99938297799636,0.570018707895176));
#15247=CARTESIAN_POINT('Ctrl Pts',(6.44573778191154,2.04546526724322,0.574245911293307));
#15248=CARTESIAN_POINT('Ctrl Pts',(6.3763007180164,2.08811202078007,0.57847311469144));
#15249=CARTESIAN_POINT('Ctrl Pts',(6.30700696413278,2.13067075638531,0.582691593634165));
#15250=CARTESIAN_POINT('Ctrl Pts',(6.23554147196038,2.16980785869403,0.586910072576891));
#15251=CARTESIAN_POINT('Ctrl Pts',(6.16227797187666,2.20530340381632,0.591128551519615));
#15252=CARTESIAN_POINT('Ctrl Pts',(6.08903849658293,2.24078730913139,0.595345647125882));
#15253=CARTESIAN_POINT('Ctrl Pts',(6.01400260215497,2.27263182628028,0.599562742732148));
#15254=CARTESIAN_POINT('Ctrl Pts',(5.93756795157103,2.30066332151541,0.603779838338415));
#15255=CARTESIAN_POINT('Ctrl Pts',(5.86113497830359,2.32869420161474,0.607996841402831));
#15256=CARTESIAN_POINT('Ctrl Pts',(5.78330374658067,2.35291206724796,0.612213844467248));
#15257=CARTESIAN_POINT('Ctrl Pts',(5.70448984443651,2.37319222362698,0.616430847531664));
#15258=CARTESIAN_POINT('Ctrl Pts',(5.62534965112499,2.39355634026833,0.620665309075044));
#15259=CARTESIAN_POINT('Ctrl Pts',(5.54521908721839,2.40994994376372,0.624899770618424));
#15260=CARTESIAN_POINT('Ctrl Pts',(5.46453034046925,2.42229837109694,0.629134232161804));
#15261=CARTESIAN_POINT('Ctrl Pts',(5.38405776682966,2.43461371577561,0.633357349165134));
#15262=CARTESIAN_POINT('Ctrl Pts',(5.30303046671959,2.44290552482371,0.637580466168465));
#15263=CARTESIAN_POINT('Ctrl Pts',(5.22188154726539,2.44715187978548,0.641803583171796));
#15264=CARTESIAN_POINT('Ctrl Pts',(5.14040564284983,2.45141534519335,0.646043716985201));
#15265=CARTESIAN_POINT('Ctrl Pts',(5.05880760837054,2.45160069338741,0.650283850798605));
#15266=CARTESIAN_POINT('Ctrl Pts',(4.97752315877383,2.44773847262252,0.65452398461201));
#15267=CARTESIAN_POINT('Ctrl Pts',(4.89623870917711,2.44387625185763,0.658764118425415));
#15268=CARTESIAN_POINT('Ctrl Pts',(4.81526830353269,2.4359665694822,0.663004252238823));
#15269=CARTESIAN_POINT('Ctrl Pts',(4.73503801466486,2.4240917066919,0.667244386052229));
#15270=CARTESIAN_POINT('Ctrl Pts',(4.65495993439779,2.41223937225435,0.67147647571119));
#15271=CARTESIAN_POINT('Ctrl Pts',(4.57532040791205,2.39639268582385,0.675708565370152));
#15272=CARTESIAN_POINT('Ctrl Pts',(4.49654862582763,2.37659601279823,0.679940655029114));
#15273=CARTESIAN_POINT('Ctrl Pts',(4.41788942743378,2.35682763394663,0.684166696021154));
#15274=CARTESIAN_POINT('Ctrl Pts',(4.34009595714993,2.33312059334035,0.688392737013193));
#15275=CARTESIAN_POINT('Ctrl Pts',(4.26358989931003,2.3055707207787,0.692618778005233));
#15276=CARTESIAN_POINT('Ctrl Pts',(4.1870627978721,2.27801327040609,0.696845981403367));
#15277=CARTESIAN_POINT('Ctrl Pts',(4.11182427435526,2.24661096831319,0.701073184801499));
#15278=CARTESIAN_POINT('Ctrl Pts',(4.03828377926988,2.2115104410777,0.705300388199633));
#15279=CARTESIAN_POINT('Ctrl Pts',(3.96489506320004,2.17648235724177,0.709518867142355));
#15280=CARTESIAN_POINT('Ctrl Pts',(3.89319780366117,2.13777147604315,0.713737346085078));
#15281=CARTESIAN_POINT('Ctrl Pts',(3.82357974791018,2.09557194427452,0.717955825027801));
#15282=CARTESIAN_POINT('Ctrl Pts',(3.75398452152405,2.05338625070485,0.722172920634062));
#15283=CARTESIAN_POINT('Ctrl Pts',(3.68646754197223,2.00771441915376,0.726390016240323));
#15284=CARTESIAN_POINT('Ctrl Pts',(3.62139071186076,1.95879584683578,0.730607111846584));
#15285=CARTESIAN_POINT('Ctrl Pts',(3.55631530982468,1.90987834800907,0.734824114910991));
#15286=CARTESIAN_POINT('Ctrl Pts',(3.49368032151808,1.85771453021222,0.739041117975399));
#15287=CARTESIAN_POINT('Ctrl Pts',(3.43381631600767,1.80258543845324,0.743258121039807));
#15288=CARTESIAN_POINT('Ctrl Pts',(3.37370447228947,1.74722811112628,0.747492582583193));
#15289=CARTESIAN_POINT('Ctrl Pts',(3.31638695987479,1.68888121508059,0.75172704412658));
#15290=CARTESIAN_POINT('Ctrl Pts',(3.26216137660341,1.62786692471803,0.755961505669966));
#15291=CARTESIAN_POINT('Ctrl Pts',(3.20808106901703,1.56701609765623,0.760184622673298));
#15292=CARTESIAN_POINT('Ctrl Pts',(3.15707640526136,1.50351254078266,0.76440773967663));
#15293=CARTESIAN_POINT('Ctrl Pts',(3.10940121141869,1.43770787110703,0.768630856679963));
#15294=CARTESIAN_POINT('Ctrl Pts',(3.06153391309053,1.37163804525283,0.772870990493376));
#15295=CARTESIAN_POINT('Ctrl Pts',(3.01702322307984,1.30324892287484,0.777111124306789));
#15296=CARTESIAN_POINT('Ctrl Pts',(2.97608034673345,1.23292282976579,0.781351258120202));
#15297=CARTESIAN_POINT('Ctrl Pts',(2.93513747038705,1.16259673665673,0.785591391933614));
#15298=CARTESIAN_POINT('Ctrl Pts',(2.89776256714275,1.09033411649246,0.789831525747029));
#15299=CARTESIAN_POINT('Ctrl Pts',(2.86411817867463,1.01653732291217,0.794071659560442));
#15300=CARTESIAN_POINT('Ctrl Pts',(2.83053761853575,0.942880532650499,0.798303749219408));
#15301=CARTESIAN_POINT('Ctrl Pts',(2.80054813471453,0.867420592882111,0.802535838878374));
#15302=CARTESIAN_POINT('Ctrl Pts',(2.77434578854549,0.790541863893586,0.80676792853734));
#15303=CARTESIAN_POINT('Ctrl Pts',(2.74818089178728,0.713773012970487,0.810993969529392));
#15304=CARTESIAN_POINT('Ctrl Pts',(2.72579253108114,0.635589836403893,0.815220010521445));
#15305=CARTESIAN_POINT('Ctrl Pts',(2.70732949048839,0.556398369082758,0.819446051513497));
#15306=CARTESIAN_POINT('Ctrl Pts',(2.68886137148995,0.477185119520685,0.823673254911629));
#15307=CARTESIAN_POINT('Ctrl Pts',(2.67432090143937,0.396963459550137,0.827900458309758));
#15308=CARTESIAN_POINT('Ctrl Pts',(2.66380757770066,0.316156767664058,0.83212766170789));
#15309=CARTESIAN_POINT('Ctrl Pts',(2.6533159522375,0.23551685137731,0.836346140650612));
#15310=CARTESIAN_POINT('Ctrl Pts',(2.64683495131427,0.154294773248336,0.840564619593335));
#15311=CARTESIAN_POINT('Ctrl Pts',(2.64441238840442,0.0729215260660757,
0.844783098536056));
#15312=CARTESIAN_POINT('Ctrl Pts',(2.64199061990878,-0.00842503695328016,
0.849000194142323));
#15313=CARTESIAN_POINT('Ctrl Pts',(2.64362466028645,-0.0899222064568432,
0.853217289748588));
#15314=CARTESIAN_POINT('Ctrl Pts',(2.64931029310321,-0.171136085285999,
0.857434385354854));
#15315=CARTESIAN_POINT('Ctrl Pts',(2.65499580115189,-0.252348181921224,
0.861651388419275));
#15316=CARTESIAN_POINT('Ctrl Pts',(2.66473269126414,-0.333276536768552,
0.865868391483699));
#15317=CARTESIAN_POINT('Ctrl Pts',(2.67846475733523,-0.413490913755362,
0.87008539454812));
#15318=CARTESIAN_POINT('Ctrl Pts',(2.69225367444079,-0.494037379903908,
0.874319856091498));
#15319=CARTESIAN_POINT('Ctrl Pts',(2.71007085127495,-0.573863476621761,
0.878554317634875));
#15320=CARTESIAN_POINT('Ctrl Pts',(2.73180763696944,-0.652544285318772,
0.882788779178253));
#15321=CARTESIAN_POINT('Ctrl Pts',(2.75348618767155,-0.731014300370378,
0.887011896181586));
#15322=CARTESIAN_POINT('Ctrl Pts',(2.77906318609869,-0.808344725248847,
0.891235013184922));
#15323=CARTESIAN_POINT('Ctrl Pts',(2.80838147504369,-0.88413137705768,0.895458130188255));
#15324=CARTESIAN_POINT('Ctrl Pts',(2.83781790036854,-0.960223406874867,
0.899698264001657));
#15325=CARTESIAN_POINT('Ctrl Pts',(2.87102563075662,-1.03475876913531,0.903938397815057));
#15326=CARTESIAN_POINT('Ctrl Pts',(2.90779856556226,-1.10735236224961,0.908178531628458));
#15327=CARTESIAN_POINT('Ctrl Pts',(2.94457150036789,-1.17994595536391,0.912418665441859));
#15328=CARTESIAN_POINT('Ctrl Pts',(2.98490935385601,-1.2505974043332,0.916658799255261));
#15329=CARTESIAN_POINT('Ctrl Pts',(3.02856276223632,-1.31895156700725,0.920898933068662));
#15330=CARTESIAN_POINT('Ctrl Pts',(3.07213335371174,-1.38717605183027,0.925131022727625));
#15331=CARTESIAN_POINT('Ctrl Pts',(3.11916947096479,-1.45336649920344,0.929363112386589));
#15332=CARTESIAN_POINT('Ctrl Pts',(3.16945507369053,-1.51714941285713,0.933595202045552));
#15333=CARTESIAN_POINT('Ctrl Pts',(3.21966880627985,-1.58084116549341,0.937821243037608));
#15334=CARTESIAN_POINT('Ctrl Pts',(3.27312251498275,-1.64213185662239,0.942047284029663));
#15335=CARTESIAN_POINT('Ctrl Pts',(3.32955626775376,-1.70067589058484,0.946273325021719));
#15336=CARTESIAN_POINT('Ctrl Pts',(3.38600554307584,-1.75923602754793,0.95050052841985));
#15337=CARTESIAN_POINT('Ctrl Pts',(3.44543622880785,-1.81504761766274,0.95472773181798));
#15338=CARTESIAN_POINT('Ctrl Pts',(3.50754704413301,-1.86779700675161,0.958954935216112));
#15339=CARTESIAN_POINT('Ctrl Pts',(3.56952966997029,-1.9204375272459,0.963173414158834));
#15340=CARTESIAN_POINT('Ctrl Pts',(3.63418103546849,-1.97002815426122,0.967391893101556));
#15341=CARTESIAN_POINT('Ctrl Pts',(3.70116537433347,-2.01629447586623,0.971610372044278));
#15342=CARTESIAN_POINT('Ctrl Pts',(3.76812774749006,-2.06254562567816,0.975827467650538));
#15343=CARTESIAN_POINT('Ctrl Pts',(3.83742119266738,-2.10547437106498,0.9800445632568));
#15344=CARTESIAN_POINT('Ctrl Pts',(3.90867922331487,-2.14484839299855,0.98426165886306));
#15345=CARTESIAN_POINT('Ctrl Pts',(3.97993569024395,-2.1842215508908,0.988478661927469));
#15346=CARTESIAN_POINT('Ctrl Pts',(4.05315624964188,-2.22003991669338,0.992695664991879));
#15347=CARTESIAN_POINT('Ctrl Pts',(4.12794922733446,-2.25211679936304,0.996912668056289));
#15348=CARTESIAN_POINT('Ctrl Pts',(4.20305184948507,-2.28432648098329,1.00114712959967));
#15349=CARTESIAN_POINT('Ctrl Pts',(4.27973950882047,-2.31276343604565,1.00538159114305));
#15350=CARTESIAN_POINT('Ctrl Pts',(4.35759648647079,-2.33728788386237,1.00961605268644));
#15351=CARTESIAN_POINT('Ctrl Pts',(4.43524487760027,-2.36174662826496,1.01383916968977));
#15352=CARTESIAN_POINT('Ctrl Pts',(4.51405586678778,-2.3823137244071,1.01806228669311));
#15353=CARTESIAN_POINT('Ctrl Pts',(4.5936047727015,-2.39890137725466,1.02228540369644));
#15354=CARTESIAN_POINT('Ctrl Pts',(4.67347421641284,-2.41555586910712,1.02652553750985));
#15355=CARTESIAN_POINT('Ctrl Pts',(4.75408706910114,-2.42819871555461,1.03076567132326));
#15356=CARTESIAN_POINT('Ctrl Pts',(4.835008060753,-2.43679357480658,1.03500580513666));
#15357=CARTESIAN_POINT('Ctrl Pts',(4.91592905240485,-2.44538843405855,1.03924593895007));
#15358=CARTESIAN_POINT('Ctrl Pts',(4.99715771294229,-2.44993534210655,1.04348607276348));
#15359=CARTESIAN_POINT('Ctrl Pts',(5.07826040200378,-2.45045055575236,1.04772620657688));
#15360=CARTESIAN_POINT('Ctrl Pts',(5.15920922739371,-2.45096479196247,1.05195829623585));
#15361=CARTESIAN_POINT('Ctrl Pts',(5.240334562324,-2.44746455166313,1.05619038589481));
#15362=CARTESIAN_POINT('Ctrl Pts',(5.32120547477968,-2.43992814441332,1.06042247555377));
#15363=CARTESIAN_POINT('Ctrl Pts',(5.40196080338606,-2.43240250848948,1.06464851654581));
#15364=CARTESIAN_POINT('Ctrl Pts',(5.48246197290976,-2.4208522055311,1.06887455753785));
#15365=CARTESIAN_POINT('Ctrl Pts',(5.56227761120284,-2.40530755216622,1.07310059852989));
#15366=CARTESIAN_POINT('Ctrl Pts',(5.64211520342029,-2.38975862312114,1.07732780192803));
#15367=CARTESIAN_POINT('Ctrl Pts',(5.72126642100674,-2.37021316962655,1.08155500532616));
#15368=CARTESIAN_POINT('Ctrl Pts',(5.79930422572347,-2.34675357746031,1.08578220872429));
#15369=CARTESIAN_POINT('Ctrl Pts',(5.87718096950144,-2.32334240315962,1.09000068766702));
#15370=CARTESIAN_POINT('Ctrl Pts',(5.95394843948697,-2.29603334055061,1.09421916660974));
#15371=CARTESIAN_POINT('Ctrl Pts',(6.02919379005196,-2.26495905236258,1.09843764555246));
#15372=CARTESIAN_POINT('Ctrl Pts',(6.10441446593258,-2.23389495414972,1.10265474115873));
#15373=CARTESIAN_POINT('Ctrl Pts',(6.17811358446272,-2.19906825960464,1.106871836765));
#15374=CARTESIAN_POINT('Ctrl Pts',(6.24989693204501,-2.16066029760598,1.11108893237127));
#15375=CARTESIAN_POINT('Ctrl Pts',(6.3216787043813,-2.12225317844887,1.1153059354357));
#15376=CARTESIAN_POINT('Ctrl Pts',(6.39154438017327,-2.08026516833278,1.11952293850013));
#15377=CARTESIAN_POINT('Ctrl Pts',(6.45912435248184,-2.03492354003424,1.12373994156455));
#15378=CARTESIAN_POINT('Ctrl Pts',(6.52698410725816,-1.98939419646706,1.12797440310793));
#15379=CARTESIAN_POINT('Ctrl Pts',(6.59253879355162,-1.940483659642,1.13220886465131));
#15380=CARTESIAN_POINT('Ctrl Pts',(6.65544510872166,-1.88846488398099,1.13644332619469));
#15381=CARTESIAN_POINT('Ctrl Pts',(6.71818289167012,-1.83658547174959,1.14066644319803));
#15382=CARTESIAN_POINT('Ctrl Pts',(6.77828615862655,-1.78161479991805,1.14488956020137));
#15383=CARTESIAN_POINT('Ctrl Pts',(6.83545036964668,-1.72386160401061,1.14911267720471));
#15384=CARTESIAN_POINT('Ctrl Pts',(6.89284492060773,-1.66587569488113,1.15335281101811));
#15385=CARTESIAN_POINT('Ctrl Pts',(6.94727637205012,-1.60508514727145,1.1575929448315));
#15386=CARTESIAN_POINT('Ctrl Pts',(6.99847761586214,-1.54183555337905,1.1618330786449));
#15387=CARTESIAN_POINT('Ctrl Pts',(7.04967885967416,-1.47858595948665,1.1660732124583));
#15388=CARTESIAN_POINT('Ctrl Pts',(7.09764967054028,-1.41287773343903,1.1703133462717));
#15389=CARTESIAN_POINT('Ctrl Pts',(7.14216797518797,-1.34508369115379,1.17455348008509));
#15390=CARTESIAN_POINT('Ctrl Pts',(7.18746672627468,-1.27610115754332,1.17886794730723));
#15391=CARTESIAN_POINT('Ctrl Pts',(7.2293551016474,-1.20470926392159,1.18318241452936));
#15392=CARTESIAN_POINT('Ctrl Pts',(7.26757389031839,-1.13127157776659,1.18749688175149));
#15393=CARTESIAN_POINT('Ctrl Pts',(7.30573175456377,-1.05795095834772,1.19180447129784));
#15394=CARTESIAN_POINT('Ctrl Pts',(7.34023145647742,-0.982591415569996,
1.19611206084419));
#15395=CARTESIAN_POINT('Ctrl Pts',(7.37085724304463,-0.90558502096874,1.20041965039054));
#15396=CARTESIAN_POINT('Ctrl Pts',(7.40143315944261,-0.828704021413996,
1.20472022557926));
#15397=CARTESIAN_POINT('Ctrl Pts',(7.42814755207704,-0.750181913787925,
1.20902080076798));
#15398=CARTESIAN_POINT('Ctrl Pts',(7.45083143436931,-0.670433500931087,
1.21332137595669));
#15399=CARTESIAN_POINT('Ctrl Pts',(7.47349353380038,-0.590761668819372,
1.21761782139235));
#15400=CARTESIAN_POINT('Ctrl Pts',(7.49213269474065,-0.50986629385648,1.221914266828));
#15401=CARTESIAN_POINT('Ctrl Pts',(7.50662893554611,-0.428179658531404,
1.22621071226366));
#15402=CARTESIAN_POINT('Ctrl Pts',(7.52111435624916,-0.346553994721007,
1.23050395080035));
#15403=CARTESIAN_POINT('Ctrl Pts',(7.53146292938334,-0.264138678010635,
1.23479718933704));
#15404=CARTESIAN_POINT('Ctrl Pts',(7.53760547669634,-0.181377414860852,
1.23909042787373));
#15405=CARTESIAN_POINT('Ctrl Pts',(7.54210976449271,-0.120689148475219,
1.24223863023382));
#15406=CARTESIAN_POINT('Ctrl Pts',(7.54435344337769,-0.0598151464494927,
1.2453868325939));
#15407=CARTESIAN_POINT('Ctrl Pts',(7.54432692296591,0.00106743604236301,
1.24853503495399));
#15408=CARTESIAN_POINT('',(7.54432671099194,0.00147590784950144,2.0485350349256));
#15409=CARTESIAN_POINT('Ctrl Pts',(7.54432692296551,0.0010674369623747,
1.24853503500156));
#15410=CARTESIAN_POINT('Ctrl Pts',(7.54428806046215,0.0902835300895766,
1.25314834645204));
#15411=CARTESIAN_POINT('Ctrl Pts',(7.5393728342159,0.17934237197442,1.25776165790251));
#15412=CARTESIAN_POINT('Ctrl Pts',(7.52965757937397,0.267731947853721,1.26237496935299));
#15413=CARTESIAN_POINT('Ctrl Pts',(7.5199136595364,0.356382318416006,1.26700189244358));
#15414=CARTESIAN_POINT('Ctrl Pts',(7.50534147059153,0.444359170624326,1.27162881553417));
#15415=CARTESIAN_POINT('Ctrl Pts',(7.48606828497608,0.531161583907084,1.27625573862477));
#15416=CARTESIAN_POINT('Ctrl Pts',(7.4667091059621,0.618351293543798,1.28090330619257));
#15417=CARTESIAN_POINT('Ctrl Pts',(7.44260702225187,0.704355770605615,1.28555087376038));
#15418=CARTESIAN_POINT('Ctrl Pts',(7.4139396961747,0.788687548010236,1.29019844132819));
#15419=CARTESIAN_POINT('Ctrl Pts',(7.39094795642238,0.856323234495913,1.2939258787499));
#15420=CARTESIAN_POINT('Ctrl Pts',(7.36502066814117,0.922883320604921,1.2976533161716));
#15421=CARTESIAN_POINT('Ctrl Pts',(7.33627098328141,0.988127486225723,1.30138075359331));
#15422=CARTESIAN_POINT('Ctrl Pts',(7.30362892112772,1.06220496289194,1.30561284325227));
#15423=CARTESIAN_POINT('Ctrl Pts',(7.26725138371584,1.13480142576407,1.30984493291123));
#15424=CARTESIAN_POINT('Ctrl Pts',(7.22729484661253,1.20551477003763,1.3140770225702));
#15425=CARTESIAN_POINT('Ctrl Pts',(7.18739541694394,1.27612704805308,1.31830306356224));
#15426=CARTESIAN_POINT('Ctrl Pts',(7.14392737370832,1.34486115174554,1.32252910455429));
#15427=CARTESIAN_POINT('Ctrl Pts',(7.09709482980959,1.41133584765583,1.32675514554634));
#15428=CARTESIAN_POINT('Ctrl Pts',(7.0502494042483,1.47782882795833,1.33098234894447));
#15429=CARTESIAN_POINT('Ctrl Pts',(7.00003783915847,1.54206074159131,1.33520955234261));
#15430=CARTESIAN_POINT('Ctrl Pts',(6.94670998865652,1.60367560822633,1.33943675574074));
#15431=CARTESIAN_POINT('Ctrl Pts',(6.89349220062614,1.6651633089538,1.34365523468346));
#15432=CARTESIAN_POINT('Ctrl Pts',(6.83717126285887,1.72404438670867,1.34787371362619));
#15433=CARTESIAN_POINT('Ctrl Pts',(6.77803710266946,1.77999637743943,1.35209219256891));
#15434=CARTESIAN_POINT('Ctrl Pts',(6.71892233393394,1.83593002022301,1.35630928817517));
#15435=CARTESIAN_POINT('Ctrl Pts',(6.65699651209806,1.88893616434786,1.36052638378143));
#15436=CARTESIAN_POINT('Ctrl Pts',(6.59258635189092,1.93872925420057,1.36474347938769));
#15437=CARTESIAN_POINT('Ctrl Pts',(6.52817760512931,1.98852125137131,1.36896048245211));
#15438=CARTESIAN_POINT('Ctrl Pts',(6.46128499673596,2.03510005115916,1.37317748551653));
#15439=CARTESIAN_POINT('Ctrl Pts',(6.39226710089324,2.0782213448248,1.37739448858095));
#15440=CARTESIAN_POINT('Ctrl Pts',(6.32296346954969,2.12152116152846,1.38162895012433));
#15441=CARTESIAN_POINT('Ctrl Pts',(6.25151730910752,2.16133452191954,1.38586341166772));
#15442=CARTESIAN_POINT('Ctrl Pts',(6.17831811948979,2.19745980598572,1.3900978732111));
#15443=CARTESIAN_POINT('Ctrl Pts',(6.10531503771946,2.23348830685345,1.39432099021443));
#15444=CARTESIAN_POINT('Ctrl Pts',(6.03056875330173,2.26584831961874,1.39854410721776));
#15445=CARTESIAN_POINT('Ctrl Pts',(5.95448556150857,2.29438823177031,1.40276722422109));
#15446=CARTESIAN_POINT('Ctrl Pts',(5.87809579681594,2.3230431438767,1.4070073580345));
#15447=CARTESIAN_POINT('Ctrl Pts',(5.8003587797785,2.34784696952838,1.41124749184791));
#15448=CARTESIAN_POINT('Ctrl Pts',(5.72169912686977,2.36869732923169,1.41548762566131));
#15449=CARTESIAN_POINT('Ctrl Pts',(5.64303947396105,2.389547688935,1.41972775947472));
#15450=CARTESIAN_POINT('Ctrl Pts',(5.56345765524226,2.40644454648053,1.42396789328813));
#15451=CARTESIAN_POINT('Ctrl Pts',(5.48338470822628,2.41933775299717,1.42820802710153));
#15452=CARTESIAN_POINT('Ctrl Pts',(5.40346367131056,2.43220649921394,1.43244011676049));
#15453=CARTESIAN_POINT('Ctrl Pts',(5.32275520129993,2.44113479794549,1.43667220641945));
#15454=CARTESIAN_POINT('Ctrl Pts',(5.24168186473874,2.4460354116288,1.44090429607841));
#15455=CARTESIAN_POINT('Ctrl Pts',(5.16072440133901,2.45092902116469,1.44513033707046));
#15456=CARTESIAN_POINT('Ctrl Pts',(5.07940356707361,2.4518063509304,1.44935637806251));
#15457=CARTESIAN_POINT('Ctrl Pts',(4.99815030471606,2.44863149335155,1.45358241905456));
#15458=CARTESIAN_POINT('Ctrl Pts',(4.9168746930044,2.44545576250295,1.45780962245269));
#15459=CARTESIAN_POINT('Ctrl Pts',(4.83566715474352,2.4382255669776,1.46203682585082));
#15460=CARTESIAN_POINT('Ctrl Pts',(4.7549623003575,2.4269571195184,1.46626402924896));
#15461=CARTESIAN_POINT('Ctrl Pts',(4.67442401139006,2.41571192882215,1.47048250819168));
#15462=CARTESIAN_POINT('Ctrl Pts',(4.59438679711928,2.40044517801082,1.4747009871344));
#15463=CARTESIAN_POINT('Ctrl Pts',(4.51527891886781,2.38122493434451,1.47891946607712));
#15464=CARTESIAN_POINT('Ctrl Pts',(4.43619698191265,2.36201099343903,1.48313656168339));
#15465=CARTESIAN_POINT('Ctrl Pts',(4.35804422697278,2.33884624391855,1.48735365728965));
#15466=CARTESIAN_POINT('Ctrl Pts',(4.28123793294673,2.31184969352821,1.49157075289591));
#15467=CARTESIAN_POINT('Ctrl Pts',(4.20443332439259,2.28485373556233,1.49578775596033));
#15468=CARTESIAN_POINT('Ctrl Pts',(4.12897555601967,2.25402629908896,1.50000475902475));
#15469=CARTESIAN_POINT('Ctrl Pts',(4.05526460406163,2.21953555431023,1.50422176208917));
#15470=CARTESIAN_POINT('Ctrl Pts',(3.98124848725441,2.18490201714246,1.50845622363255));
#15471=CARTESIAN_POINT('Ctrl Pts',(3.90899411417661,2.14657496300712,1.51269068517593));
#15472=CARTESIAN_POINT('Ctrl Pts',(3.83888244061972,2.10477172460857,1.51692514671931));
#15473=CARTESIAN_POINT('Ctrl Pts',(3.76895860315021,2.06308048120803,1.52114826372264));
#15474=CARTESIAN_POINT('Ctrl Pts',(3.70116636520278,2.01793194928828,1.52537138072598));
#15475=CARTESIAN_POINT('Ctrl Pts',(3.63585383805487,1.96958474195826,1.52959449772931));
#15476=CARTESIAN_POINT('Ctrl Pts',(3.5702781377889,1.92104272230266,1.53383463154272));
#15477=CARTESIAN_POINT('Ctrl Pts',(3.50720253317648,1.86927650081015,1.53807476535612));
#15478=CARTESIAN_POINT('Ctrl Pts',(3.44694377047309,1.81458683073496,1.54231489916953));
#15479=CARTESIAN_POINT('Ctrl Pts',(3.3866850077697,1.75989716065978,1.54655503298293));
#15480=CARTESIAN_POINT('Ctrl Pts',(3.32924337288416,1.70228441686834,1.55079516679634));
#15481=CARTESIAN_POINT('Ctrl Pts',(3.27489526229107,1.64208313371704,1.55503530060974));
#15482=CARTESIAN_POINT('Ctrl Pts',(3.22065025801833,1.58199606121111,1.5592673902687));
#15483=CARTESIAN_POINT('Ctrl Pts',(3.16928466213748,1.51910610009245,1.56349947992767));
#15484=CARTESIAN_POINT('Ctrl Pts',(3.12110139711795,1.45372051385435,1.56773156958663));
#15485=CARTESIAN_POINT('Ctrl Pts',(3.07298699749225,1.38842837923572,1.57195761057867));
#15486=CARTESIAN_POINT('Ctrl Pts',(3.02804616865433,1.32064807460014,1.57618365157072));
#15487=CARTESIAN_POINT('Ctrl Pts',(2.9865433020495,1.25072179607794,1.58040969256277));
#15488=CARTESIAN_POINT('Ctrl Pts',(2.94502901975208,1.18077628377831,1.5846368959609));
#15489=CARTESIAN_POINT('Ctrl Pts',(2.90695488381131,1.10868398065176,1.58886409935903));
#15490=CARTESIAN_POINT('Ctrl Pts',(2.87254353178807,1.03481849289501,1.59309130275716));
#15491=CARTESIAN_POINT('Ctrl Pts',(2.83820320078702,0.961105454900816,1.59730978169989));
#15492=CARTESIAN_POINT('Ctrl Pts',(2.80751076859186,0.885626954952128,1.60152826064261));
#15493=CARTESIAN_POINT('Ctrl Pts',(2.78064189706716,0.808779457198272,1.60574673958533));
#15494=CARTESIAN_POINT('Ctrl Pts',(2.75378183646462,0.731957159509874,1.6099638351916));
#15495=CARTESIAN_POINT('Ctrl Pts',(2.73074299978355,0.653767193853023,1.61418093079786));
#15496=CARTESIAN_POINT('Ctrl Pts',(2.71165232180658,0.574624496468033,1.61839802640412));
#15497=CARTESIAN_POINT('Ctrl Pts',(2.69256206276406,0.495483535826052,1.62261502946854));
#15498=CARTESIAN_POINT('Ctrl Pts',(2.677419898011,0.415390337026596,1.62683203253295));
#15499=CARTESIAN_POINT('Ctrl Pts',(2.6663020920874,0.334772036961452,1.63104903559737));
#15500=CARTESIAN_POINT('Ctrl Pts',(2.65513825821981,0.253819975484603,1.63528349714075));
#15501=CARTESIAN_POINT('Ctrl Pts',(2.64803225323112,0.172338921240921,1.63951795868414));
#15502=CARTESIAN_POINT('Ctrl Pts',(2.6450087376301,0.0907667699699964,1.64375242022752));
#15503=CARTESIAN_POINT('Ctrl Pts',(2.64199332232552,0.00941315853642459,
1.64797553723085));
#15504=CARTESIAN_POINT('Ctrl Pts',(2.64303850239018,-0.0720305954233467,
1.65219865423419));
#15505=CARTESIAN_POINT('Ctrl Pts',(2.64811643569602,-0.153131725208311,
1.65642177123752));
#15506=CARTESIAN_POINT('Ctrl Pts',(2.65321483024568,-0.234559647388847,
1.66066190505093));
#15507=CARTESIAN_POINT('Ctrl Pts',(2.66237848463236,-0.315641710899356,
1.66490203886433));
#15508=CARTESIAN_POINT('Ctrl Pts',(2.67552713668527,-0.395948568917046,
1.66914217267774));
#15509=CARTESIAN_POINT('Ctrl Pts',(2.68867578873818,-0.476255426934736,
1.67338230649115));
#15510=CARTESIAN_POINT('Ctrl Pts',(2.70580927922514,-0.555786635709915,
1.67762244030455));
#15511=CARTESIAN_POINT('Ctrl Pts',(2.72679705821168,-0.634128353532026,
1.68186257411796));
#15512=CARTESIAN_POINT('Ctrl Pts',(2.74774502030965,-0.712321445649074,
1.68609466377692));
#15513=CARTESIAN_POINT('Ctrl Pts',(2.7726107971626,-0.789621282590697,1.69032675343589));
#15514=CARTESIAN_POINT('Ctrl Pts',(2.8013011478423,-0.865606581784154,1.69455884309485));
#15515=CARTESIAN_POINT('Ctrl Pts',(2.82995049315847,-0.941483279836695,
1.6987848840869));
#15516=CARTESIAN_POINT('Ctrl Pts',(2.86241339300268,-1.01604874051948,1.70301092507894));
#15517=CARTESIAN_POINT('Ctrl Pts',(2.8985463407754,-1.08889503383382,1.70723696607099));
#15518=CARTESIAN_POINT('Ctrl Pts',(2.93468922720193,-1.16176136409881,1.71146416946912));
#15519=CARTESIAN_POINT('Ctrl Pts',(2.97450403450885,-1.23290713780912,1.71569137286725));
#15520=CARTESIAN_POINT('Ctrl Pts',(3.0177981952346,-1.30194239747158,1.71991857626539));
#15521=CARTESIAN_POINT('Ctrl Pts',(3.06100300185571,-1.37083517639963,1.72413705520811));
#15522=CARTESIAN_POINT('Ctrl Pts',(3.10767258855501,-1.43762573730366,1.72835553415083));
#15523=CARTESIAN_POINT('Ctrl Pts',(3.15756966680859,-1.50195112692391,1.73257401309355));
#15524=CARTESIAN_POINT('Ctrl Pts',(3.20745038266034,-1.56625542276655,1.73679110869982));
#15525=CARTESIAN_POINT('Ctrl Pts',(3.26055620364706,-1.62809578581825,1.74100820430608));
#15526=CARTESIAN_POINT('Ctrl Pts',(3.31660784946631,-1.68714012116001,1.74522529991234));
#15527=CARTESIAN_POINT('Ctrl Pts',(3.37265826526298,-1.74618316080625,1.74944230297676));
#15528=CARTESIAN_POINT('Ctrl Pts',(3.43165405659566,-1.80242995851394,1.75365930604117));
#15529=CARTESIAN_POINT('Ctrl Pts',(3.49327815909478,-1.8555843177437,1.75787630910559));
#15530=CARTESIAN_POINT('Ctrl Pts',(3.55515738663906,-1.90895873710819,1.76211077064897));
#15531=CARTESIAN_POINT('Ctrl Pts',(3.61968638538108,-1.95921474002239,1.76634523219235));
#15532=CARTESIAN_POINT('Ctrl Pts',(3.68651100948259,-2.00609359584509,1.77057969373574));
#15533=CARTESIAN_POINT('Ctrl Pts',(3.75315660382636,-2.05284685859018,1.77480281073907));
#15534=CARTESIAN_POINT('Ctrl Pts',(3.82208512119671,-2.09624083229109,1.77902592774241));
#15535=CARTESIAN_POINT('Ctrl Pts',(3.89291818142928,-2.13606364280399,1.78324904474574));
#15536=CARTESIAN_POINT('Ctrl Pts',(3.96403665945441,-2.17604691706972,1.78748917855914));
#15537=CARTESIAN_POINT('Ctrl Pts',(4.03707463540398,-2.21242998530242,1.79172931237255));
#15538=CARTESIAN_POINT('Ctrl Pts',(4.11162810508851,-2.24504683146318,1.79596944618596));
#15539=CARTESIAN_POINT('Ctrl Pts',(4.18618157477305,-2.27766367762394,1.80020957999936));
#15540=CARTESIAN_POINT('Ctrl Pts',(4.26225007917263,-2.30651419415162,1.80444971381277));
#15541=CARTESIAN_POINT('Ctrl Pts',(4.33941529296309,-2.33148300266897,1.80868984762617));
#15542=CARTESIAN_POINT('Ctrl Pts',(4.41643411304883,-2.35640444170205,1.81292193728513));
#15543=CARTESIAN_POINT('Ctrl Pts',(4.49483282171878,-2.37755187957483,1.81715402694409));
#15544=CARTESIAN_POINT('Ctrl Pts',(4.5742071285654,-2.3947745776288,1.82138611660305));
#15545=CARTESIAN_POINT('Ctrl Pts',(4.65346799056975,-2.41197266033378,1.8256121575951));
#15546=CARTESIAN_POINT('Ctrl Pts',(4.73370123106809,-2.42525704636647,1.82983819858715));
#15547=CARTESIAN_POINT('Ctrl Pts',(4.81448644377937,-2.43452644610848,1.83406423957919));
#15548=CARTESIAN_POINT('Ctrl Pts',(4.89529387710404,-2.4437983954724,1.83829144297732));
#15549=CARTESIAN_POINT('Ctrl Pts',(4.97665313471908,-2.44905303133571,1.84251864637546));
#15550=CARTESIAN_POINT('Ctrl Pts',(5.0581322271524,-2.45024001316067,1.84674584977359));
#15551=CARTESIAN_POINT('Ctrl Pts',(5.13944315623,-2.45142454519341,1.85096432871632));
#15552=CARTESIAN_POINT('Ctrl Pts',(5.22087296166411,-2.44855816498041,1.85518280765904));
#15553=CARTESIAN_POINT('Ctrl Pts',(5.30198801066615,-2.44164274789679,1.85940128660176));
#15554=CARTESIAN_POINT('Ctrl Pts',(5.38307646017434,-2.43472959853779,1.86361838220803));
#15555=CARTESIAN_POINT('Ctrl Pts',(5.46384989557651,-2.42377008858649,1.86783547781429));
#15556=CARTESIAN_POINT('Ctrl Pts',(5.54387775932526,-2.40881811350594,1.87205257342056));
#15557=CARTESIAN_POINT('Ctrl Pts',(5.62390386690647,-2.39386646653827,1.87626957648497));
#15558=CARTESIAN_POINT('Ctrl Pts',(5.70318397879108,-2.37492261511094,1.88048657954939));
#15559=CARTESIAN_POINT('Ctrl Pts',(5.78129713029502,-2.35209168267116,1.88470358261381));
#15560=CARTESIAN_POINT('Ctrl Pts',(5.85973367184437,-2.32916622970396,1.88893804415719));
#15561=CARTESIAN_POINT('Ctrl Pts',(5.93699311348128,-2.30232156197435,1.89317250570057));
#15562=CARTESIAN_POINT('Ctrl Pts',(6.01266578101148,-2.27171429325565,1.89740696724395));
#15563=CARTESIAN_POINT('Ctrl Pts',(6.08813571400305,-2.24118902442812,1.90163008424729));
#15564=CARTESIAN_POINT('Ctrl Pts',(6.1620269574203,-2.20692152369229,1.90585320125062));
#15565=CARTESIAN_POINT('Ctrl Pts',(6.23395599308187,-2.16911421635821,1.91007631825396));
#15566=CARTESIAN_POINT('Ctrl Pts',(6.30617486270674,-2.13115456662685,1.91431645206736));
#15567=CARTESIAN_POINT('Ctrl Pts',(6.37641527654647,-2.0896267705324,1.91855658588077));
#15568=CARTESIAN_POINT('Ctrl Pts',(6.4443182790114,-2.04477968866826,1.92279671969418));
#15569=CARTESIAN_POINT('Ctrl Pts',(6.51222128147632,-1.99993260680413,1.92703685350758));
#15570=CARTESIAN_POINT('Ctrl Pts',(6.57778653276988,-1.95176656598368,1.93127698732099));
#15571=CARTESIAN_POINT('Ctrl Pts',(6.64068979568123,-1.90056997299928,1.9355171211344));
#15572=CARTESIAN_POINT('Ctrl Pts',(6.70265595672201,-1.85013608167505,1.93969408751985));
#15573=CARTESIAN_POINT('Ctrl Pts',(6.76228324590583,-1.79656223509988,1.9438710539053));
#15574=CARTESIAN_POINT('Ctrl Pts',(6.81923004557809,-1.74009629525161,1.94804802029075));
#15575=CARTESIAN_POINT('Ctrl Pts',(6.8763130790926,-1.68349527192215,1.95223497923387));
#15576=CARTESIAN_POINT('Ctrl Pts',(6.93070236814598,-1.62398855423777,1.95642193817699));
#15577=CARTESIAN_POINT('Ctrl Pts',(6.98208507709209,-1.56186819910249,1.96060889712011));
#15578=CARTESIAN_POINT('Ctrl Pts',(7.0332127811925,-1.50005613817552,1.9647750768003));
#15579=CARTESIAN_POINT('Ctrl Pts',(7.08136334922856,-1.43565667276066,1.96894125648049));
#15580=CARTESIAN_POINT('Ctrl Pts',(7.1262649478876,-1.36899483924668,1.97310743616068));
#15581=CARTESIAN_POINT('Ctrl Pts',(7.17113945057062,-1.30237323297396,1.97727110174988));
#15582=CARTESIAN_POINT('Ctrl Pts',(7.21276860737517,-1.23349236269156,1.98143476733907));
#15583=CARTESIAN_POINT('Ctrl Pts',(7.25092218098948,-1.16270860528605,1.98559843292827));
#15584=CARTESIAN_POINT('Ctrl Pts',(7.28906513501693,-1.09194454968535,1.98976093961139));
#15585=CARTESIAN_POINT('Ctrl Pts',(7.32373420028611,-1.01927907926499,1.99392344629451));
#15586=CARTESIAN_POINT('Ctrl Pts',(7.35474445735159,-0.945094283114693,
1.99808595297763));
#15587=CARTESIAN_POINT('Ctrl Pts',(7.38606450716415,-0.870168380183437,
2.00229004313996));
#15588=CARTESIAN_POINT('Ctrl Pts',(7.4136520138649,-0.793693069530683,2.00649413330229));
#15589=CARTESIAN_POINT('Ctrl Pts',(7.43736645441978,-0.716082260776532,
2.01069822346462));
#15590=CARTESIAN_POINT('Ctrl Pts',(7.46086810650685,-0.639167849858183,
2.01486459053995));
#15591=CARTESIAN_POINT('Ctrl Pts',(7.48056585136317,-0.561138719230198,
2.01903095761529));
#15592=CARTESIAN_POINT('Ctrl Pts',(7.49637378505751,-0.482410553964721,
2.02319732469062));
#15593=CARTESIAN_POINT('Ctrl Pts',(7.5123964108495,-0.402613158825682,2.02742027639645));
#15594=CARTESIAN_POINT('Ctrl Pts',(7.52442268876795,-0.322098098698069,
2.03164322810228));
#15595=CARTESIAN_POINT('Ctrl Pts',(7.53241743836409,-0.241304127797537,
2.03586617980811));
#15596=CARTESIAN_POINT('Ctrl Pts',(7.54041218796023,-0.160510156897006,
2.04008913151394));
#15597=CARTESIAN_POINT('Ctrl Pts',(7.54437544438211,-0.079437782649294,
2.04431208321977));
#15598=CARTESIAN_POINT('Ctrl Pts',(7.54432671099194,0.00147590784949135,
2.0485350349256));
#15599=CARTESIAN_POINT('',(7.54432621659511,-0.002145073936182,2.84853503499689));
#15600=CARTESIAN_POINT('Ctrl Pts',(7.54432671099162,0.00147590839337491,
2.04853503495399));
#15601=CARTESIAN_POINT('Ctrl Pts',(7.54427359039347,0.0896737956893433,
2.0531381548502));
#15602=CARTESIAN_POINT('Ctrl Pts',(7.53945915089848,0.17772660136509,2.0577412747464));
#15603=CARTESIAN_POINT('Ctrl Pts',(7.52992837234614,0.265256688986949,2.0623443946426));
#15604=CARTESIAN_POINT('Ctrl Pts',(7.52116581341596,0.345731494558948,2.06657648430155));
#15605=CARTESIAN_POINT('Ctrl Pts',(7.5083949867179,0.425921753537977,2.0708085739605));
#15606=CARTESIAN_POINT('Ctrl Pts',(7.49164371171518,0.505396886135544,2.07504066361945));
#15607=CARTESIAN_POINT('Ctrl Pts',(7.47491637828531,0.584758429786803,2.07926670461149));
#15608=CARTESIAN_POINT('Ctrl Pts',(7.4542199905826,0.663406426132384,2.08349274560353));
#15609=CARTESIAN_POINT('Ctrl Pts',(7.42963408316964,0.740915816021938,2.08771878659557));
#15610=CARTESIAN_POINT('Ctrl Pts',(7.40504141320785,0.81844652548394,2.0919459899937));
#15611=CARTESIAN_POINT('Ctrl Pts',(7.37655716042474,0.894837541586089,2.09617319339183));
#15612=CARTESIAN_POINT('Ctrl Pts',(7.34431208924527,0.969674075540071,2.10040039678997));
#15613=CARTESIAN_POINT('Ctrl Pts',(7.31213356813673,1.04435615560513,2.10461887573268));
#15614=CARTESIAN_POINT('Ctrl Pts',(7.27620989784197,1.1174897269735,2.1088373546754));
#15615=CARTESIAN_POINT('Ctrl Pts',(7.23672016284678,1.18867985970291,2.11305583361812));
#15616=CARTESIAN_POINT('Ctrl Pts',(7.1972433774457,1.25984664754727,2.11727292922438));
#15617=CARTESIAN_POINT('Ctrl Pts',(7.1542030748911,1.32907085632596,2.12149002483064));
#15618=CARTESIAN_POINT('Ctrl Pts',(7.10782455095711,1.39598164060389,2.1257071204369));
#15619=CARTESIAN_POINT('Ctrl Pts',(7.06144704477438,1.46289095656135,2.12992412350132));
#15620=CARTESIAN_POINT('Ctrl Pts',(7.01173172852818,1.52748656769599,2.13414112656573));
#15621=CARTESIAN_POINT('Ctrl Pts',(6.9589467205048,1.58942733651507,2.13835812963014));
#15622=CARTESIAN_POINT('Ctrl Pts',(6.90594318146806,1.65162454138457,2.14259259117353));
#15623=CARTESIAN_POINT('Ctrl Pts',(6.84984477555372,1.71114450745861,2.14682705271692));
#15624=CARTESIAN_POINT('Ctrl Pts',(6.79096198855441,1.76767746160725,2.15106151426031));
#15625=CARTESIAN_POINT('Ctrl Pts',(6.73223695434822,1.82405895839669,2.15528463126365));
#15626=CARTESIAN_POINT('Ctrl Pts',(6.67074281928052,1.87746915229913,2.15950774826698));
#15627=CARTESIAN_POINT('Ctrl Pts',(6.60682117406737,1.92764087672924,2.16373086527032));
#15628=CARTESIAN_POINT('Ctrl Pts',(6.54264196021563,1.97801476527315,2.16797099908374));
#15629=CARTESIAN_POINT('Ctrl Pts',(6.47601602181197,2.02512376565215,2.17221113289716));
#15630=CARTESIAN_POINT('Ctrl Pts',(6.40731727544797,2.06874211893989,2.17645126671058));
#15631=CARTESIAN_POINT('Ctrl Pts',(6.33861852908397,2.11236047222762,2.180691400524));
#15632=CARTESIAN_POINT('Ctrl Pts',(6.26784741197262,2.15248800203392,2.18493153433742));
#15633=CARTESIAN_POINT('Ctrl Pts',(6.19539972605475,2.18894680650264,2.18917166815084));
#15634=CARTESIAN_POINT('Ctrl Pts',(6.12308948400096,2.22533644328293,2.1934037578098));
#15635=CARTESIAN_POINT('Ctrl Pts',(6.04883926109604,2.25820703877901,2.19763584746876));
#15636=CARTESIAN_POINT('Ctrl Pts',(5.97302558958405,2.28734788858663,2.20186793712773));
#15637=CARTESIAN_POINT('Ctrl Pts',(5.89732027391604,2.31644708915984,2.20609397811977));
#15638=CARTESIAN_POINT('Ctrl Pts',(5.82005637780858,2.34182696605905,2.21032001911182));
#15639=CARTESIAN_POINT('Ctrl Pts',(5.74163391104989,2.36332322321835,2.21454606010386));
#15640=CARTESIAN_POINT('Ctrl Pts',(5.66318987356978,2.38482539309366,2.21877326350199));
#15641=CARTESIAN_POINT('Ctrl Pts',(5.58358705627131,2.40244162072258,2.22300046690013));
#15642=CARTESIAN_POINT('Ctrl Pts',(5.50324469600782,2.41605619294878,2.22722767029826));
#15643=CARTESIAN_POINT('Ctrl Pts',(5.42306815301729,2.42964266628378,2.23144614924098));
#15644=CARTESIAN_POINT('Ctrl Pts',(5.34215557068417,2.43924388332878,2.2356646281837));
#15645=CARTESIAN_POINT('Ctrl Pts',(5.26093578305467,2.44479548358981,2.23988310712642));
#15646=CARTESIAN_POINT('Ctrl Pts',(5.17974262926524,2.45034526335317,2.24410020273269));
#15647=CARTESIAN_POINT('Ctrl Pts',(5.09824293348796,2.45184803188112,2.24831729833895));
#15648=CARTESIAN_POINT('Ctrl Pts',(5.01687043383599,2.44929130831715,2.25253439394521));
#15649=CARTESIAN_POINT('Ctrl Pts',(4.93549971985879,2.44673464085907,2.25675139700962));
#15650=CARTESIAN_POINT('Ctrl Pts',(4.85425666088054,2.44011867417226,2.26096840007404));
#15651=CARTESIAN_POINT('Ctrl Pts',(4.77357333693884,2.42948301943583,2.26518540313846));
#15652=CARTESIAN_POINT('Ctrl Pts',(4.69255598238529,2.41880333287118,2.26941986468184));
#15653=CARTESIAN_POINT('Ctrl Pts',(4.61210347680974,2.40407065306822,2.27365432622522));
#15654=CARTESIAN_POINT('Ctrl Pts',(4.53264460451389,2.38537720172751,2.2778887877686));
#15655=CARTESIAN_POINT('Ctrl Pts',(4.45339861037261,2.36673383198636,2.28211190477194));
#15656=CARTESIAN_POINT('Ctrl Pts',(4.3751413700557,2.34415105539868,2.28633502177527));
#15657=CARTESIAN_POINT('Ctrl Pts',(4.29828281380327,2.31777036189285,2.2905581387786));
#15658=CARTESIAN_POINT('Ctrl Pts',(4.22111456036433,2.29128336888108,2.29479827259201));
#15659=CARTESIAN_POINT('Ctrl Pts',(4.14535672112151,2.26096797051491,2.29903840640541));
#15660=CARTESIAN_POINT('Ctrl Pts',(4.07140204223235,2.22701529807397,2.30327854021882));
#15661=CARTESIAN_POINT('Ctrl Pts',(3.99744736334318,2.19306262563304,2.30751867403222));
#15662=CARTESIAN_POINT('Ctrl Pts',(3.92529623052251,2.15547295021277,2.31175880784563));
#15663=CARTESIAN_POINT('Ctrl Pts',(3.85531311721876,2.11448178689164,2.31599894165903));
#15664=CARTESIAN_POINT('Ctrl Pts',(3.78546277212388,2.07356838980691,2.320231031318));
#15665=CARTESIAN_POINT('Ctrl Pts',(3.71751162249775,2.02911377346404,2.32446312097696));
#15666=CARTESIAN_POINT('Ctrl Pts',(3.65184120019895,1.98131944795627,2.32869521063593));
#15667=CARTESIAN_POINT('Ctrl Pts',(3.58626463661834,1.93359343195486,2.33292125162797));
#15668=CARTESIAN_POINT('Ctrl Pts',(3.52296269881717,1.88253745812461,2.33714729262002));
#15669=CARTESIAN_POINT('Ctrl Pts',(3.46229072743443,1.82839796927475,2.34137333361207));
#15670=CARTESIAN_POINT('Ctrl Pts',(3.40160206774487,1.77424358892919,2.3456005370102));
#15671=CARTESIAN_POINT('Ctrl Pts',(3.34354521018637,1.71700425552848,2.34982774040833));
#15672=CARTESIAN_POINT('Ctrl Pts',(3.28844516845862,1.65696895898379,2.35405494380647));
#15673=CARTESIAN_POINT('Ctrl Pts',(3.23345884679868,1.59705756829797,2.35827342274919));
#15674=CARTESIAN_POINT('Ctrl Pts',(3.18141748076242,1.53436206949908,2.36249190169191));
#15675=CARTESIAN_POINT('Ctrl Pts',(3.13260819768634,1.46920742228462,2.36671038063464));
#15676=CARTESIAN_POINT('Ctrl Pts',(3.08381492029897,1.40407414078046,2.3709274762409));
#15677=CARTESIAN_POINT('Ctrl Pts',(3.03825189944832,1.33648368393925,2.37514457184717));
#15678=CARTESIAN_POINT('Ctrl Pts',(2.99616538269479,1.26679332849066,2.37936166745343));
#15679=CARTESIAN_POINT('Ctrl Pts',(2.95407978950675,1.19710450235861,2.38357867051785));
#15680=CARTESIAN_POINT('Ctrl Pts',(2.91547078796965,1.12531626761467,2.38779567358227));
#15681=CARTESIAN_POINT('Ctrl Pts',(2.880540000536,1.0518128254965,2.39201267664669));
#15682=CARTESIAN_POINT('Ctrl Pts',(2.84546459892773,0.978005077624156,2.39624713819007));
#15683=CARTESIAN_POINT('Ctrl Pts',(2.81409814620306,0.902468310741889,2.40048159973345));
#15684=CARTESIAN_POINT('Ctrl Pts',(2.78659631431134,0.825612557852792,2.40471606127683));
#15685=CARTESIAN_POINT('Ctrl Pts',(2.75916816253928,0.748962709104628,2.40893917828017));
#15686=CARTESIAN_POINT('Ctrl Pts',(2.73558404662123,0.671001392178894,2.41316229528351));
#15687=CARTESIAN_POINT('Ctrl Pts',(2.71594803617511,0.592149596049576,2.41738541228684));
#15688=CARTESIAN_POINT('Ctrl Pts',(2.69623290354033,0.512980071086965,2.42162554610025));
#15689=CARTESIAN_POINT('Ctrl Pts',(2.68049784333027,0.4329133397623,2.42586567991365));
#15690=CARTESIAN_POINT('Ctrl Pts',(2.668795917416,0.352382951551585,2.43010581372705));
#15691=CARTESIAN_POINT('Ctrl Pts',(2.65709399150174,0.271852563340869,2.43434594754046));
#15692=CARTESIAN_POINT('Ctrl Pts',(2.64942518200458,0.190858989358771,2.43858608135386));
#15693=CARTESIAN_POINT('Ctrl Pts',(2.64578992844836,0.109836174363986,2.44282621516727));
#15694=CARTESIAN_POINT('Ctrl Pts',(2.64216157150021,0.0289670715079627,
2.44705830482623));
#15695=CARTESIAN_POINT('Ctrl Pts',(2.6425379274089,-0.0522328669521755,
2.45129039448519));
#15696=CARTESIAN_POINT('Ctrl Pts',(2.6469572506401,-0.133333862616963,2.45552248414415));
#15697=CARTESIAN_POINT('Ctrl Pts',(2.65137025760289,-0.214318945588759,
2.4597485251362));
#15698=CARTESIAN_POINT('Ctrl Pts',(2.65981473035322,-0.295204906503504,
2.46397456612824));
#15699=CARTESIAN_POINT('Ctrl Pts',(2.67227697172963,-0.375559526185646,
2.46820060712029));
#15700=CARTESIAN_POINT('Ctrl Pts',(2.68474264094436,-0.455936248043137,
2.47242781051842));
#15701=CARTESIAN_POINT('Ctrl Pts',(2.70122828366821,-0.535780869538314,
2.47665501391656));
#15702=CARTESIAN_POINT('Ctrl Pts',(2.72166800539679,-0.614663498838233,
2.48088221731469));
#15703=CARTESIAN_POINT('Ctrl Pts',(2.74206554192063,-0.693383323579882,
2.48510069625741));
#15704=CARTESIAN_POINT('Ctrl Pts',(2.76640075986744,-0.771144666907021,
2.48931917520013));
#15705=CARTESIAN_POINT('Ctrl Pts',(2.7945569789483,-0.847529884685807,2.49353765414286));
#15706=CARTESIAN_POINT('Ctrl Pts',(2.82270396495606,-0.923890053991391,
2.49775474974912));
#15707=CARTESIAN_POINT('Ctrl Pts',(2.85466930317223,-0.998874558242367,
2.50197184535538));
#15708=CARTESIAN_POINT('Ctrl Pts',(2.89028696632634,-1.07208249911243,2.50618894096164));
#15709=CARTESIAN_POINT('Ctrl Pts',(2.92590384787039,-1.14528883347444,2.51040594402606));
#15710=CARTESIAN_POINT('Ctrl Pts',(2.96517269066384,-1.21671826461455,2.51462294709048));
#15711=CARTESIAN_POINT('Ctrl Pts',(3.00788061081696,-1.28599271495624,2.51883995015489));
#15712=CARTESIAN_POINT('Ctrl Pts',(3.05076534263331,-1.35555396293968,2.52307441169827));
#15713=CARTESIAN_POINT('Ctrl Pts',(3.09711745153451,-1.42294194041319,2.52730887324165));
#15714=CARTESIAN_POINT('Ctrl Pts',(3.14667739375335,-1.48780309702345,2.53154333478503));
#15715=CARTESIAN_POINT('Ctrl Pts',(3.19610455999973,-1.552490484199,2.53576645178837));
#15716=CARTESIAN_POINT('Ctrl Pts',(3.24872205982453,-1.61466424210871,2.5399895687917));
#15717=CARTESIAN_POINT('Ctrl Pts',(3.30423310345922,-1.6740081777184,2.54421268579504));
#15718=CARTESIAN_POINT('Ctrl Pts',(3.35996782569094,-1.73359123634561,2.54845281960844));
#15719=CARTESIAN_POINT('Ctrl Pts',(3.41861911483808,-1.79032129774357,2.55269295342185));
#15720=CARTESIAN_POINT('Ctrl Pts',(3.47985191156118,-1.84391815493638,2.55693308723525));
#15721=CARTESIAN_POINT('Ctrl Pts',(3.54108470828428,-1.89751501212919,2.56117322104866));
#15722=CARTESIAN_POINT('Ctrl Pts',(3.60489860743148,-1.94797842403459,2.56541335486206));
#15723=CARTESIAN_POINT('Ctrl Pts',(3.6709296133877,-1.99507213773944,2.56965348867547));
#15724=CARTESIAN_POINT('Ctrl Pts',(3.73683534886111,-2.0420765077766,2.57388557833443));
#15725=CARTESIAN_POINT('Ctrl Pts',(3.80519565810401,-2.08589933025433,2.57811766799339));
#15726=CARTESIAN_POINT('Ctrl Pts',(3.8756705980363,-2.12627487677921,2.58234975765236));
#15727=CARTESIAN_POINT('Ctrl Pts',(3.94604481244714,-2.16659271700477,2.5865757986444));
#15728=CARTESIAN_POINT('Ctrl Pts',(4.01852725507039,-2.20347283772714,2.59080183963645));
#15729=CARTESIAN_POINT('Ctrl Pts',(4.0927476942418,-2.2366917897513,2.59502788062849));
#15730=CARTESIAN_POINT('Ctrl Pts',(4.1669885483336,-2.26991987891165,2.59925508402663));
#15731=CARTESIAN_POINT('Ctrl Pts',(4.24296796032467,-2.29948453604172,2.60348228742476));
#15732=CARTESIAN_POINT('Ctrl Pts',(4.32028927855364,-2.3252073892455,2.60770949082289));
#15733=CARTESIAN_POINT('Ctrl Pts',(4.39745101458852,-2.35087715347658,2.61192796976561));
#15734=CARTESIAN_POINT('Ctrl Pts',(4.47594869025042,-2.37272078559758,2.61614644870834));
#15735=CARTESIAN_POINT('Ctrl Pts',(4.55536832789653,-2.39060919872454,2.62036492765106));
#15736=CARTESIAN_POINT('Ctrl Pts',(4.63476192201321,-2.40849174582859,2.62458202325732));
#15737=CARTESIAN_POINT('Ctrl Pts',(4.71507642472786,-2.42242154764815,2.62879911886358));
#15738=CARTESIAN_POINT('Ctrl Pts',(4.79588509004015,-2.43232003972698,2.63301621446985));
#15739=CARTESIAN_POINT('Ctrl Pts',(4.87669198205073,-2.44221831458884,2.63723321753426));
#15740=CARTESIAN_POINT('Ctrl Pts',(4.957992553717,-2.44808540024345,2.64145022059868));
#15741=CARTESIAN_POINT('Ctrl Pts',(5.03935374343876,-2.44989446658086,2.6456672236631));
#15742=CARTESIAN_POINT('Ctrl Pts',(5.12105177015058,-2.45171102248992,2.64990168520648));
#15743=CARTESIAN_POINT('Ctrl Pts',(5.20281044650658,-2.44943586357772,2.65413614674986));
#15744=CARTESIAN_POINT('Ctrl Pts',(5.28419193459196,-2.44309465655005,2.65837060829325));
#15745=CARTESIAN_POINT('Ctrl Pts',(5.36535539364545,-2.43677043824134,2.66259372529658));
#15746=CARTESIAN_POINT('Ctrl Pts',(5.44614322436628,-2.42640203104198,2.66681684229992));
#15747=CARTESIAN_POINT('Ctrl Pts',(5.52612869875607,-2.41206667106402,2.67103995930325));
#15748=CARTESIAN_POINT('Ctrl Pts',(5.60643647007138,-2.39767354756735,2.67528009311666));
#15749=CARTESIAN_POINT('Ctrl Pts',(5.68593494793452,-2.37928154924512,2.67952022693006));
#15750=CARTESIAN_POINT('Ctrl Pts',(5.76420680689366,-2.35701959536497,2.68376036074347));
#15751=CARTESIAN_POINT('Ctrl Pts',(5.84247866585281,-2.33475764148481,2.68800049455688));
#15752=CARTESIAN_POINT('Ctrl Pts',(5.91952348332117,-2.30862594106609,2.69224062837029));
#15753=CARTESIAN_POINT('Ctrl Pts',(5.99494509779225,-2.27880159381954,2.6964807621837));
#15754=CARTESIAN_POINT('Ctrl Pts',(6.07022362642169,-2.24903382772491,2.70071285184266));
#15755=CARTESIAN_POINT('Ctrl Pts',(6.14416596005127,-2.21547637032557,2.70494494150162));
#15756=CARTESIAN_POINT('Ctrl Pts',(6.21636427122024,-2.17827011036859,2.70917703116058));
#15757=CARTESIAN_POINT('Ctrl Pts',(6.28845939375874,-2.14111702704343,2.71340307215263));
#15758=CARTESIAN_POINT('Ctrl Pts',(6.35881503484576,-2.10032570982552,2.71762911314467));
#15759=CARTESIAN_POINT('Ctrl Pts',(6.42704239006815,-2.05608545255064,2.72185515413672));
#15760=CARTESIAN_POINT('Ctrl Pts',(6.49528851176561,-2.01183302664219,2.72608235753485));
#15761=CARTESIAN_POINT('Ctrl Pts',(6.56140475299464,-1.96412995919919,2.73030956093299));
#15762=CARTESIAN_POINT('Ctrl Pts',(6.62502578388396,-1.91321222301434,2.73453676433112));
#15763=CARTESIAN_POINT('Ctrl Pts',(6.68851550837637,-1.86239957510586,2.73875524327384));
#15764=CARTESIAN_POINT('Ctrl Pts',(6.74951993344176,-1.80838578546842,2.74297372221657));
#15765=CARTESIAN_POINT('Ctrl Pts',(6.80770567885512,-1.75144815995831,2.74719220115929));
#15766=CARTESIAN_POINT('Ctrl Pts',(6.86587234382169,-1.6945292056077,2.75140929676555));
#15767=CARTESIAN_POINT('Ctrl Pts',(6.92122183286099,-1.63468864421221,2.75562639237181));
#15768=CARTESIAN_POINT('Ctrl Pts',(6.97345623146411,-1.57224196185385,2.75984348797808));
#15769=CARTESIAN_POINT('Ctrl Pts',(7.02568948381206,-1.50979664985361,2.7640604910425));
#15770=CARTESIAN_POINT('Ctrl Pts',(7.07480748437652,-1.44474568777084,2.76827749410692));
#15771=CARTESIAN_POINT('Ctrl Pts',(7.1205523091914,-1.37743798452217,2.77249449717133));
#15772=CARTESIAN_POINT('Ctrl Pts',(7.16648651851691,-1.309851626005,2.77672895871472));
#15773=CARTESIAN_POINT('Ctrl Pts',(7.20901928670969,-1.23999018358204,2.78096342025809));
#15774=CARTESIAN_POINT('Ctrl Pts',(7.24793415705625,-1.16823511145844,2.78519788180148));
#15775=CARTESIAN_POINT('Ctrl Pts',(7.28674477062765,-1.09667227824904,2.78942099880481));
#15776=CARTESIAN_POINT('Ctrl Pts',(7.3219566819964,-1.02322638824702,2.79364411580814));
#15777=CARTESIAN_POINT('Ctrl Pts',(7.35340275872267,-0.948297602606365,
2.79786723281148));
#15778=CARTESIAN_POINT('Ctrl Pts',(7.38497554562883,-0.873066895680292,
2.80210736662488));
#15779=CARTESIAN_POINT('Ctrl Pts',(7.41275193301665,-0.796341763627506,
2.80634750043829));
#15780=CARTESIAN_POINT('Ctrl Pts',(7.4366132801029,-0.718542569475471,2.81058763425169));
#15781=CARTESIAN_POINT('Ctrl Pts',(7.46047462718915,-0.640743375323441,
2.8148277680651));
#15782=CARTESIAN_POINT('Ctrl Pts',(7.48042087970566,-0.561870587392187,
2.8190679018785));
#15783=CARTESIAN_POINT('Ctrl Pts',(7.49638534176926,-0.482352994564428,
2.82330803569191));
#15784=CARTESIAN_POINT('Ctrl Pts',(7.51922595399613,-0.368585897636371,
2.82937446322553));
#15785=CARTESIAN_POINT('Ctrl Pts',(7.53399165590758,-0.253147670603014,
2.83544089075915));
#15786=CARTESIAN_POINT('Ctrl Pts',(7.54049542395752,-0.136984064378373,
2.84150731829277));
#15787=CARTESIAN_POINT('Ctrl Pts',(7.5430068767487,-0.0921270813424802,
2.84384989051318));
#15788=CARTESIAN_POINT('Ctrl Pts',(7.54428681030232,-0.0471621918703228,
2.84619246273358));
#15789=CARTESIAN_POINT('Ctrl Pts',(7.54432621659438,-0.00214507476057291,
2.84853503495399));
#15790=CARTESIAN_POINT('',(7.54393141126483,8.94937218200234E-5,3.64853504140039));
#15791=CARTESIAN_POINT('Ctrl Pts',(7.54432621659511,-0.0021450739361722,
2.84853503499689));
#15792=CARTESIAN_POINT('Ctrl Pts',(7.54439742906591,0.0792069437731955,
2.85276837975536));
#15793=CARTESIAN_POINT('Ctrl Pts',(7.54041302387129,0.160689976852925,2.85700172451383));
#15794=CARTESIAN_POINT('Ctrl Pts',(7.53236234262213,0.241860271517619,2.86123506927229));
#15795=CARTESIAN_POINT('Ctrl Pts',(7.52445196900469,0.321615926668091,2.86539463510958));
#15796=CARTESIAN_POINT('Ctrl Pts',(7.51261596087071,0.401069158613188,2.86955420094686));
#15797=CARTESIAN_POINT('Ctrl Pts',(7.49689665975846,0.47979913242696,2.87371376678415));
#15798=CARTESIAN_POINT('Ctrl Pts',(7.48118511182867,0.558490274498245,2.87787128101158));
#15799=CARTESIAN_POINT('Ctrl Pts',(7.4615941642831,0.636458396846369,2.88202879523902));
#15800=CARTESIAN_POINT('Ctrl Pts',(7.4382176456193,0.713290599698551,2.88618630946646));
#15801=CARTESIAN_POINT('Ctrl Pts',(7.4148450175322,0.790110015292633,2.89034313175476));
#15802=CARTESIAN_POINT('Ctrl Pts',(7.38768820935883,0.86579342840745,2.89449995404307));
#15803=CARTESIAN_POINT('Ctrl Pts',(7.35689109022833,0.93994248607013,2.89865677633138));
#15804=CARTESIAN_POINT('Ctrl Pts',(7.32510818814065,1.01646497603422,2.90294665407044));
#15805=CARTESIAN_POINT('Ctrl Pts',(7.28944814638991,1.09135270273379,2.9072365318095));
#15806=CARTESIAN_POINT('Ctrl Pts',(7.2501222516031,1.16419143972094,2.91152640954857));
#15807=CARTESIAN_POINT('Ctrl Pts',(7.21196864925906,1.23485887707526,2.9156884073937));
#15808=CARTESIAN_POINT('Ctrl Pts',(7.17036499723827,1.30359738498866,2.91985040523883));
#15809=CARTESIAN_POINT('Ctrl Pts',(7.12554925654204,1.3700567703372,2.92401240308397));
#15810=CARTESIAN_POINT('Ctrl Pts',(7.07866802985336,1.43957916273128,2.92836622077));
#15811=CARTESIAN_POINT('Ctrl Pts',(7.028271843264,1.50660680265626,2.93272003845602));
#15812=CARTESIAN_POINT('Ctrl Pts',(6.97467977651935,1.57077804537378,2.93707385614205));
#15813=CARTESIAN_POINT('Ctrl Pts',(6.9210877097747,1.6349492880913,2.94142767382807));
#15814=CARTESIAN_POINT('Ctrl Pts',(6.86430022451701,1.69626375536157,2.9457814915141));
#15815=CARTESIAN_POINT('Ctrl Pts',(6.80467773584327,1.75440603669123,2.95013530920012));
#15816=CARTESIAN_POINT('Ctrl Pts',(6.7467222273782,1.81092272280643,2.95436739885909));
#15817=CARTESIAN_POINT('Ctrl Pts',(6.6858551205809,1.86466997352527,2.95859948851805));
#15818=CARTESIAN_POINT('Ctrl Pts',(6.62237179651115,1.91533326872707,2.96283157817702));
#15819=CARTESIAN_POINT('Ctrl Pts',(6.55897920527397,1.96592415397953,2.96705761916906));
#15820=CARTESIAN_POINT('Ctrl Pts',(6.49297818339017,2.01343955046757,2.9712836601611));
#15821=CARTESIAN_POINT('Ctrl Pts',(6.42470050117019,2.05760209653369,2.97550970115314));
#15822=CARTESIAN_POINT('Ctrl Pts',(6.35640403863222,2.10177678985834,2.97973690455128));
#15823=CARTESIAN_POINT('Ctrl Pts',(6.28583001538864,2.14259648168644,2.98396410794941));
#15824=CARTESIAN_POINT('Ctrl Pts',(6.21334319503753,2.17982432482831,2.98819131134754));
#15825=CARTESIAN_POINT('Ctrl Pts',(6.14100597904003,2.21697533403841,2.99240979029027));
#15826=CARTESIAN_POINT('Ctrl Pts',(6.0667642555964,2.25054907152295,2.99662826923299));
#15827=CARTESIAN_POINT('Ctrl Pts',(5.99100743671978,2.28035475154772,3.00084674817572));
#15828=CARTESIAN_POINT('Ctrl Pts',(5.91527546024984,2.31015065760316,3.00506384378198));
#15829=CARTESIAN_POINT('Ctrl Pts',(5.83802980710525,2.3361807900522,3.00928093938825));
#15830=CARTESIAN_POINT('Ctrl Pts',(5.7596802224845,2.35830234345066,3.01349803499451));
#15831=CARTESIAN_POINT('Ctrl Pts',(5.68133235720246,2.38042341140376,3.01771503805893));
#15832=CARTESIAN_POINT('Ctrl Pts',(5.60188105612782,2.39863594568312,3.02193204112334));
#15833=CARTESIAN_POINT('Ctrl Pts',(5.52175020561148,2.41284730414984,3.02614904418776));
#15834=CARTESIAN_POINT('Ctrl Pts',(5.44128761173451,2.42711749793138,3.03038350573114));
#15835=CARTESIAN_POINT('Ctrl Pts',(5.36014029203784,2.4373532203585,3.03461796727452));
#15836=CARTESIAN_POINT('Ctrl Pts',(5.27874486921614,2.44351298116803,3.0388524288179));
#15837=CARTESIAN_POINT('Ctrl Pts',(5.19756751275883,2.44965623937091,3.04307554582124));
#15838=CARTESIAN_POINT('Ctrl Pts',(5.11614384934191,2.45174537703917,3.04729866282457));
#15839=CARTESIAN_POINT('Ctrl Pts',(5.03490739645519,2.44979156501112,3.05152177982791));
#15840=CARTESIAN_POINT('Ctrl Pts',(4.95334360589618,2.44782988020849,3.05576191364131));
#15841=CARTESIAN_POINT('Ctrl Pts',(4.8719690072782,2.4417926387357,3.06000204745472));
#15842=CARTESIAN_POINT('Ctrl Pts',(4.79121571760324,2.43174352423985,3.06424218126812));
#15843=CARTESIAN_POINT('Ctrl Pts',(4.71046242792827,2.42169440974399,3.06848231508153));
#15844=CARTESIAN_POINT('Ctrl Pts',(4.6303308967439,2.4076335642661,3.07272244889494));
#15845=CARTESIAN_POINT('Ctrl Pts',(4.55123968223925,2.38967551854041,3.07696258270834));
#15846=CARTESIAN_POINT('Ctrl Pts',(4.4722985153445,2.37175154185586,3.08119467236731));
#15847=CARTESIAN_POINT('Ctrl Pts',(4.394099204526,2.34987828336001,3.08542676202628));
#15848=CARTESIAN_POINT('Ctrl Pts',(4.31706630786371,2.32413270611904,3.08965885168525));
#15849=CARTESIAN_POINT('Ctrl Pts',(4.2401435096094,2.29842392545705,3.09388489267729));
#15850=CARTESIAN_POINT('Ctrl Pts',(4.1643842515435,2.26885396417144,3.09811093366934));
#15851=CARTESIAN_POINT('Ctrl Pts',(4.09020168302746,2.23555052752077,3.10233697466138));
#15852=CARTESIAN_POINT('Ctrl Pts',(4.01599871000768,2.20223793049575,3.10656417805951));
#15853=CARTESIAN_POINT('Ctrl Pts',(3.94337374263367,2.16518993309172,3.11079138145764));
#15854=CARTESIAN_POINT('Ctrl Pts',(3.87272385868278,2.124583956594,3.11501858485578));
#15855=CARTESIAN_POINT('Ctrl Pts',(3.8022197878627,2.08406178610179,3.1192370637985));
#15856=CARTESIAN_POINT('Ctrl Pts',(3.73368307129303,2.03999651825496,3.12345554274123));
#15857=CARTESIAN_POINT('Ctrl Pts',(3.66748552315288,1.99261130127456,3.12767402168395));
#15858=CARTESIAN_POINT('Ctrl Pts',(3.60130968271429,1.9452416229988,3.13189111729022));
#15859=CARTESIAN_POINT('Ctrl Pts',(3.53747186494676,1.89455442789271,3.13610821289648));
#15860=CARTESIAN_POINT('Ctrl Pts',(3.47631466416858,1.8408160121366,3.14032530850274));
#15861=CARTESIAN_POINT('Ctrl Pts',(3.41515880545153,1.78707877564047,3.14454231156717));
#15862=CARTESIAN_POINT('Ctrl Pts',(3.35668379508049,1.73029075921571,3.14875931463159));
#15863=CARTESIAN_POINT('Ctrl Pts',(3.30119780931436,1.67075739632124,3.15297631769601));
#15864=CARTESIAN_POINT('Ctrl Pts',(3.24548211043202,1.61097756408647,3.15721077923939));
#15865=CARTESIAN_POINT('Ctrl Pts',(3.19278056921847,1.54842994173943,3.16144524078277));
#15866=CARTESIAN_POINT('Ctrl Pts',(3.14336535048291,1.48345845824964,3.16567970232615));
#15867=CARTESIAN_POINT('Ctrl Pts',(3.09408251999131,1.41866103977113,3.16990281932948));
#15868=CARTESIAN_POINT('Ctrl Pts',(3.04806865587466,1.35145314016491,3.17412593633281));
#15869=CARTESIAN_POINT('Ctrl Pts',(3.00555003355331,1.28220470758373,3.17834905333615));
#15870=CARTESIAN_POINT('Ctrl Pts',(2.9628600848586,1.21267724237716,3.18258918714955));
#15871=CARTESIAN_POINT('Ctrl Pts',(2.9236938239047,1.14109318278484,3.18682932096295));
#15872=CARTESIAN_POINT('Ctrl Pts',(2.8882326878449,1.06784984639978,3.19106945477635));
#15873=CARTESIAN_POINT('Ctrl Pts',(2.85277155178509,0.99460651001471,3.19530958858976));
#15874=CARTESIAN_POINT('Ctrl Pts',(2.82101566576165,0.919704351378521,3.19954972240316));
#15875=CARTESIAN_POINT('Ctrl Pts',(2.79309641776494,0.843556946896211,3.20378985621656));
#15876=CARTESIAN_POINT('Ctrl Pts',(2.76523013666798,0.767554005185249,3.20802194587553));
#15877=CARTESIAN_POINT('Ctrl Pts',(2.74108197119413,0.690026992125537,3.2122540355345));
#15878=CARTESIAN_POINT('Ctrl Pts',(2.72081810344039,0.61137409911254,3.21648612519346));
#15879=CARTESIAN_POINT('Ctrl Pts',(2.70058319759349,0.53283361986914,3.22071216618551));
#15880=CARTESIAN_POINT('Ctrl Pts',(2.68422167837404,0.453170902855609,3.22493820717756));
#15881=CARTESIAN_POINT('Ctrl Pts',(2.67185093551005,0.372802145957223,3.22916424816961));
#15882=CARTESIAN_POINT('Ctrl Pts',(2.65947678997514,0.292411282995037,3.23339145156774));
#15883=CARTESIAN_POINT('Ctrl Pts',(2.65109575197378,0.211314438421757,3.23761865496587));
#15884=CARTESIAN_POINT('Ctrl Pts',(2.64677474554041,0.129941345000103,3.241845858364));
#15885=CARTESIAN_POINT('Ctrl Pts',(2.64246265716099,0.048736196164606,3.24606433730672));
#15886=CARTESIAN_POINT('Ctrl Pts',(2.64219390782992,-0.0327435996276477,
3.25028281624944));
#15887=CARTESIAN_POINT('Ctrl Pts',(2.64598330755778,-0.11406465850992,3.25450129519216));
#15888=CARTESIAN_POINT('Ctrl Pts',(2.64977146465415,-0.195359050343041,
3.25871839079843));
#15889=CARTESIAN_POINT('Ctrl Pts',(2.65761510642675,-0.276494344813367,
3.26293548640469));
#15890=CARTESIAN_POINT('Ctrl Pts',(2.66947694299597,-0.357038229548362,
3.26715258201096));
#15891=CARTESIAN_POINT('Ctrl Pts',(2.68133851926371,-0.437580346792089,
3.27136958507538));
#15892=CARTESIAN_POINT('Ctrl Pts',(2.69721804616655,-0.517530620542038,
3.2755865881398));
#15893=CARTESIAN_POINT('Ctrl Pts',(2.71702667468682,-0.596464353192318,
3.27980359120422));
#15894=CARTESIAN_POINT('Ctrl Pts',(2.73691731133442,-0.675724873110627,
3.2840380527476));
#15895=CARTESIAN_POINT('Ctrl Pts',(2.76076954967438,-0.753959956249378,
3.28827251429097));
#15896=CARTESIAN_POINT('Ctrl Pts',(2.78844265408719,-0.830754206045222,
3.29250697583435));
#15897=CARTESIAN_POINT('Ctrl Pts',(2.81604161952438,-0.907342716472999,
3.29673009283769));
#15898=CARTESIAN_POINT('Ctrl Pts',(2.84744078598369,-0.982497688404951,
3.30095320984103));
#15899=CARTESIAN_POINT('Ctrl Pts',(2.88245263387824,-1.0558280993275,3.30517632684436));
#15900=CARTESIAN_POINT('Ctrl Pts',(2.91760556002501,-1.12945399097527,3.30941646065776));
#15901=CARTESIAN_POINT('Ctrl Pts',(2.9564001115301,-1.20124017598565,3.31365659447117));
#15902=CARTESIAN_POINT('Ctrl Pts',(2.99860142286126,-1.27081838965485,3.31789672828457));
#15903=CARTESIAN_POINT('Ctrl Pts',(3.04080273419242,-1.34039660332405,3.32213686209797));
#15904=CARTESIAN_POINT('Ctrl Pts',(3.08641049185188,-1.407766493533,3.32637699591137));
#15905=CARTESIAN_POINT('Ctrl Pts',(3.13514897760215,-1.47259296671226,3.33061712972477));
#15906=CARTESIAN_POINT('Ctrl Pts',(3.1837949993115,-1.5372964545838,3.33484921938374));
#15907=CARTESIAN_POINT('Ctrl Pts',(3.23574135673279,-1.59970757218609,3.3390813090427));
#15908=CARTESIAN_POINT('Ctrl Pts',(3.29074415854742,-1.65947038427012,3.34331339870166));
#15909=CARTESIAN_POINT('Ctrl Pts',(3.34566834822122,-1.71914778102173,3.3475394396937));
#15910=CARTESIAN_POINT('Ctrl Pts',(3.40363999413734,-1.77618405073565,3.35176548068574));
#15911=CARTESIAN_POINT('Ctrl Pts',(3.46437356851543,-1.83025442439458,3.35599152167778));
#15912=CARTESIAN_POINT('Ctrl Pts',(3.52512384814491,-1.88433967053869,3.36021872507591));
#15913=CARTESIAN_POINT('Ctrl Pts',(3.58863727450732,-1.93545703226086,3.36444592847404));
#15914=CARTESIAN_POINT('Ctrl Pts',(3.65458952705235,-1.98331674197425,3.36867313187218));
#15915=CARTESIAN_POINT('Ctrl Pts',(3.72040566183053,-2.0310776748217,3.3728916108149));
#15916=CARTESIAN_POINT('Ctrl Pts',(3.78865020450101,-2.0755940958847,3.37711008975762));
#15917=CARTESIAN_POINT('Ctrl Pts',(3.8589674417565,-2.11661799517276,3.38132856870035));
#15918=CARTESIAN_POINT('Ctrl Pts',(3.92926162036955,-2.15762844177891,3.38554566430662));
#15919=CARTESIAN_POINT('Ctrl Pts',(4.00162674271203,-2.19514840704296,3.38976275991289));
#15920=CARTESIAN_POINT('Ctrl Pts',(4.07567967434794,-2.22897419382083,3.39397985551915));
#15921=CARTESIAN_POINT('Ctrl Pts',(4.14973098093277,-2.2627992383103,3.39819685858357));
#15922=CARTESIAN_POINT('Ctrl Pts',(4.22546960001136,-2.29293007346957,3.40241386164798));
#15923=CARTESIAN_POINT('Ctrl Pts',(4.30249076210233,-2.31921041791352,3.4066308647124));
#15924=CARTESIAN_POINT('Ctrl Pts',(4.37983079338029,-2.34559956352118,3.41086532625578));
#15925=CARTESIAN_POINT('Ctrl Pts',(4.45846356743373,-2.36810610373114,3.41509978779916));
#15926=CARTESIAN_POINT('Ctrl Pts',(4.53796391712025,-2.38662236440332,3.41933424934254));
#15927=CARTESIAN_POINT('Ctrl Pts',(4.61725127753017,-2.40508901818721,3.42355736634588));
#15928=CARTESIAN_POINT('Ctrl Pts',(4.69740110343072,-2.41958670312452,3.42778048334921));
#15929=CARTESIAN_POINT('Ctrl Pts',(4.77798325534482,-2.43006026278452,3.43200360035255));
#15930=CARTESIAN_POINT('Ctrl Pts',(4.85889010846263,-2.44057602505823,3.43624373416596));
#15931=CARTESIAN_POINT('Ctrl Pts',(4.94023230836447,-2.44703513490168,3.44048386797936));
#15932=CARTESIAN_POINT('Ctrl Pts',(5.02157308115603,-2.44943454673675,3.44472400179277));
#15933=CARTESIAN_POINT('Ctrl Pts',(5.10291385394758,-2.45183395857182,3.44896413560618));
#15934=CARTESIAN_POINT('Ctrl Pts',(5.18425273366396,-2.45017374412986,3.45320426941959));
#15935=CARTESIAN_POINT('Ctrl Pts',(5.26515858208952,-2.4445031790216,3.45744440323299));
#15936=CARTESIAN_POINT('Ctrl Pts',(5.34591094027892,-2.43884337180533,3.46167649289195));
#15937=CARTESIAN_POINT('Ctrl Pts',(5.42653318044008,-2.42916731676783,3.46590858255091));
#15938=CARTESIAN_POINT('Ctrl Pts',(5.50659397124848,-2.41548624624073,3.47014067220987));
#15939=CARTESIAN_POINT('Ctrl Pts',(5.58654033606505,-2.40182472923102,3.47436671320191));
#15940=CARTESIAN_POINT('Ctrl Pts',(5.66592639105071,-2.38416964308185,3.47859275419396));
#15941=CARTESIAN_POINT('Ctrl Pts',(5.74432433169587,-2.3625841093388,3.482818795186));
#15942=CARTESIAN_POINT('Ctrl Pts',(5.82274383631637,-2.3409926383235,3.48704599858413));
#15943=CARTESIAN_POINT('Ctrl Pts',(5.9001742198754,-2.31546861631229,3.49127320198227));
#15944=CARTESIAN_POINT('Ctrl Pts',(5.97619596955483,-2.28612675193234,3.4955004053804));
#15945=CARTESIAN_POINT('Ctrl Pts',(6.05206081919819,-2.25684544574263,3.49971888432312));
#15946=CARTESIAN_POINT('Ctrl Pts',(6.12652240111848,-2.22376218462051,3.50393736326584));
#15947=CARTESIAN_POINT('Ctrl Pts',(6.19917918752779,-2.18704072554408,3.50815584220856));
#15948=CARTESIAN_POINT('Ctrl Pts',(6.27181214810253,-2.1503313082803,3.51237293781482));
#15949=CARTESIAN_POINT('Ctrl Pts',(6.34264107408638,-2.10998627179487,3.51659003342108));
#15950=CARTESIAN_POINT('Ctrl Pts',(6.4112867263889,-2.06621647678787,3.52080712902735));
#15951=CARTESIAN_POINT('Ctrl Pts',(6.47993087230009,-2.02244764228511,3.52502413209175));
#15952=CARTESIAN_POINT('Ctrl Pts',(6.5463914485901,-1.97525444948679,3.52924113515616));
#15953=CARTESIAN_POINT('Ctrl Pts',(6.61031725452029,-1.9248916929093,3.53345813822056));
#15954=CARTESIAN_POINT('Ctrl Pts',(6.67450771459521,-1.87432043348895,3.53769259976395));
#15955=CARTESIAN_POINT('Ctrl Pts',(6.73614199302411,-1.82055359212623,3.54192706130733));
#15956=CARTESIAN_POINT('Ctrl Pts',(6.79489860012048,-1.76388950621553,3.54616152285072));
#15957=CARTESIAN_POINT('Ctrl Pts',(6.85349779247216,-1.70737722897892,3.55038463985405));
#15958=CARTESIAN_POINT('Ctrl Pts',(6.90923442299243,-1.64798358050816,3.55460775685739));
#15959=CARTESIAN_POINT('Ctrl Pts',(6.96182838023185,-1.58603961937434,3.55883087386072));
#15960=CARTESIAN_POINT('Ctrl Pts',(7.01463426183454,-1.52384605856767,3.56307100767413));
#15961=CARTESIAN_POINT('Ctrl Pts',(7.06427181029833,-1.45908196846079,3.56731114148755));
#15962=CARTESIAN_POINT('Ctrl Pts',(7.11050104743682,-1.39211230272247,3.57155127530096));
#15963=CARTESIAN_POINT('Ctrl Pts',(7.15673028457532,-1.32514263698415,3.57579140911438));
#15964=CARTESIAN_POINT('Ctrl Pts',(7.19955101730721,-1.25596782571705,3.5800315429278));
#15965=CARTESIAN_POINT('Ctrl Pts',(7.23877024704368,-1.18497653303257,3.58427167674121));
#15966=CARTESIAN_POINT('Ctrl Pts',(7.27979763224545,-1.11071227209454,3.58870729682959));
#15967=CARTESIAN_POINT('Ctrl Pts',(7.31702493902605,-1.03420556025214,3.59314291691798));
#15968=CARTESIAN_POINT('Ctrl Pts',(7.35021345270096,-0.95586145836733,3.59757853700636));
#15969=CARTESIAN_POINT('Ctrl Pts',(7.38331144713053,-0.877731034294349,
3.60200205926515));
#15970=CARTESIAN_POINT('Ctrl Pts',(7.41239243550695,-0.797773568688574,
3.60642558152394));
#15971=CARTESIAN_POINT('Ctrl Pts',(7.43726394308904,-0.716417666137985,
3.61084910378273));
#15972=CARTESIAN_POINT('Ctrl Pts',(7.46209503840575,-0.635193954059309,
3.6152654385176));
#15973=CARTESIAN_POINT('Ctrl Pts',(7.48273014165557,-0.552576704786469,
3.61968177325247));
#15974=CARTESIAN_POINT('Ctrl Pts',(7.49902488252049,-0.469014012274587,
3.62409810798735));
#15975=CARTESIAN_POINT('Ctrl Pts',(7.51528614811596,-0.38562298764449,3.62850536997928));
#15976=CARTESIAN_POINT('Ctrl Pts',(7.52722473537349,-0.301290779277856,
3.63291263197121));
#15977=CARTESIAN_POINT('Ctrl Pts',(7.53474649504544,-0.216478700116522,
3.63731989396313));
#15978=CARTESIAN_POINT('Ctrl Pts',(7.54112669174313,-0.144538386813589,
3.64105827429342));
#15979=CARTESIAN_POINT('Ctrl Pts',(7.54432979256689,-0.0722532055566229,
3.6447966546237));
#15980=CARTESIAN_POINT('Ctrl Pts',(7.54432715382295,8.93836134977417E-5,
3.64853503495399));
#15981=CARTESIAN_POINT('',(7.54548616237095,0.00208864728292292,4.44853503495399));
#15982=CARTESIAN_POINT('Ctrl Pts',(7.54033669847616,9.04938866648818E-5,
3.64853509995607));
#15983=CARTESIAN_POINT('Ctrl Pts',(7.54046775454349,0.402997660035618,3.66938971672052));
#15984=CARTESIAN_POINT('Ctrl Pts',(7.2558289127575,1.62248954264943,3.73252009132105));
#15985=CARTESIAN_POINT('Ctrl Pts',(5.33475743839734,2.88488253211185,3.83792622375765));
#15986=CARTESIAN_POINT('Ctrl Pts',(2.80334611963393,1.77039296481798,3.96475349726585));
#15987=CARTESIAN_POINT('Ctrl Pts',(2.36277430168313,-0.960179636963284,
4.09158077077408));
#15988=CARTESIAN_POINT('Ctrl Pts',(4.41521294580189,-2.81426320371486,4.21840804428229));
#15989=CARTESIAN_POINT('Ctrl Pts',(6.92189640647373,-2.1435844429306,4.33739279900894));
#15990=CARTESIAN_POINT('Ctrl Pts',(7.5395029472068,-0.659618059205427,4.4141017958995));
#15991=CARTESIAN_POINT('Ctrl Pts',(7.54548616237095,0.00208864728292292,
4.44853503495399));
#15992=CARTESIAN_POINT('',(7.5469083499403,-0.00161708351646295,5.248535034954));
#15993=CARTESIAN_POINT('Ctrl Pts',(7.54548616237095,0.00208864728292292,
4.44853503495399));
#15994=CARTESIAN_POINT('Ctrl Pts',(7.54684890019601,0.152799048512293,4.45637755373557));
#15995=CARTESIAN_POINT('Ctrl Pts',(7.46563602800205,1.11446190020873,4.50649583035324));
#15996=CARTESIAN_POINT('Ctrl Pts',(6.1942094107571,2.67763954212219,4.59888986480693));
#15997=CARTESIAN_POINT('Ctrl Pts',(3.44447846030825,2.37912662696793,4.72571713831517));
#15998=CARTESIAN_POINT('Ctrl Pts',(2.20033666274626,-0.0911449062707706,
4.85254441182336));
#15999=CARTESIAN_POINT('Ctrl Pts',(3.59748467407956,-2.47821585092194,4.97937168533159));
#16000=CARTESIAN_POINT('Ctrl Pts',(6.36055186041318,-2.60307570907344,5.1061989588398));
#16001=CARTESIAN_POINT('Ctrl Pts',(7.49721259379224,-1.01042400560164,5.19592007538061));
#16002=CARTESIAN_POINT('Ctrl Pts',(7.54766539424022,-0.100812118607445,
5.24336543408534));
#16003=CARTESIAN_POINT('Ctrl Pts',(7.5469083499403,-0.00161708351646295,
5.248535034954));
#16004=CARTESIAN_POINT('',(7.54409000407149,-0.000907487779776068,6.04853499257024));
#16005=CARTESIAN_POINT('Ctrl Pts',(7.5469083499403,-0.00161708351646295,
5.248535034954));
#16006=CARTESIAN_POINT('Ctrl Pts',(7.54147446725997,0.710381122145878,5.28564119192141));
#16007=CARTESIAN_POINT('Ctrl Pts',(6.84050798882477,2.24289643598352,5.36502310672491));
#16008=CARTESIAN_POINT('Ctrl Pts',(4.2394355735632,2.76597354472522,5.48668077936444));
#16009=CARTESIAN_POINT('Ctrl Pts',(2.30775737354188,0.786390358311311,5.61350805287268));
#16010=CARTESIAN_POINT('Ctrl Pts',(2.91931121122073,-1.91104030140742,5.74033532638088));
#16011=CARTESIAN_POINT('Ctrl Pts',(5.5158471379227,-2.86399960888975,5.86716259988912));
#16012=CARTESIAN_POINT('Ctrl Pts',(7.30705098429824,-1.51821911474262,5.96989561711511));
#16013=CARTESIAN_POINT('Ctrl Pts',(7.54182188154817,-0.352067409384865,
6.03035287650504));
#16014=CARTESIAN_POINT('Ctrl Pts',(7.54065403856044,-0.000918084752164947,
6.0485343780589));
#16015=CARTESIAN_POINT('',(7.5443261628818,0.00220558177830445,6.84853503499609));
#16016=CARTESIAN_POINT('Ctrl Pts',(7.54432698768978,-0.000906756890932275,
6.04853503495399));
#16017=CARTESIAN_POINT('Ctrl Pts',(7.54435782807605,0.082439024249153,6.05284397718214));
#16018=CARTESIAN_POINT('Ctrl Pts',(7.54013222037993,0.165757790068247,6.05715291941028));
#16019=CARTESIAN_POINT('Ctrl Pts',(7.53168467216413,0.248598025365387,6.06146186163843));
#16020=CARTESIAN_POINT('Ctrl Pts',(7.5232318680157,0.331489802563786,6.06577348482317));
#16021=CARTESIAN_POINT('Ctrl Pts',(7.51055194191658,0.413902023722049,6.07008510800791));
#16022=CARTESIAN_POINT('Ctrl Pts',(7.49373099221601,0.495390577515068,6.07439673119265));
#16023=CARTESIAN_POINT('Ctrl Pts',(7.4768816418065,0.577016717635823,6.07871563417771));
#16024=CARTESIAN_POINT('Ctrl Pts',(7.45587739507284,0.65771564883538,6.08303453716278));
#16025=CARTESIAN_POINT('Ctrl Pts',(7.43085500839885,0.737055672629838,6.08735344014785));
#16026=CARTESIAN_POINT('Ctrl Pts',(7.40580967646488,0.81646845037444,6.09167630352059));
#16027=CARTESIAN_POINT('Ctrl Pts',(7.37673901636462,0.894519430353428,6.09599916689333));
#16028=CARTESIAN_POINT('Ctrl Pts',(7.34382811427782,0.97079654680468,6.10032203026608));
#16029=CARTESIAN_POINT('Ctrl Pts',(7.31084909359608,1.0472315407272,6.10465384105018));
#16030=CARTESIAN_POINT('Ctrl Pts',(7.27401414562568,1.12188494603015,6.10898565183427));
#16031=CARTESIAN_POINT('Ctrl Pts',(7.2335545487697,1.19436884264894,6.11331746261837));
#16032=CARTESIAN_POINT('Ctrl Pts',(7.21020525229535,1.23619941248367,6.11581735738076));
#16033=CARTESIAN_POINT('Ctrl Pts',(7.18564959734903,1.27730796117,6.11831725214315));
#16034=CARTESIAN_POINT('Ctrl Pts',(7.15993834715027,1.31762467855749,6.12081714690554));
#16035=CARTESIAN_POINT('Ctrl Pts',(7.11641158845541,1.38587713674324,6.1250492365645));
#16036=CARTESIAN_POINT('Ctrl Pts',(7.06941799814007,1.45209778396879,6.12928132622347));
#16037=CARTESIAN_POINT('Ctrl Pts',(7.01917337655042,1.51591298526872,6.13351341588243));
#16038=CARTESIAN_POINT('Ctrl Pts',(6.96900056652541,1.5796369794044,6.13773945687448));
#16039=CARTESIAN_POINT('Ctrl Pts',(6.91558623874065,1.64096199371702,6.14196549786652));
#16040=CARTESIAN_POINT('Ctrl Pts',(6.85919010319566,1.69954226565206,6.14619153885857));
#16041=CARTESIAN_POINT('Ctrl Pts',(6.8027784554464,1.75813865055541,6.15041874225671));
#16042=CARTESIAN_POINT('Ctrl Pts',(6.7433836323815,1.81398840427749,6.15464594565484));
#16043=CARTESIAN_POINT('Ctrl Pts',(6.68130671328082,1.86677767917852,6.15887314905297));
#16044=CARTESIAN_POINT('Ctrl Pts',(6.61935791371017,1.91945800316528,6.16309162799569));
#16045=CARTESIAN_POINT('Ctrl Pts',(6.5547384159393,1.96909014855915,6.16731010693841));
#16046=CARTESIAN_POINT('Ctrl Pts',(6.48778380992542,2.01539948780691,6.17152858588114));
#16047=CARTESIAN_POINT('Ctrl Pts',(6.42085115986981,2.06169364115514,6.1757456814874));
#16048=CARTESIAN_POINT('Ctrl Pts',(6.35158530413794,2.10466688812076,6.17996277709366));
#16049=CARTESIAN_POINT('Ctrl Pts',(6.28035257997533,2.14408667431202,6.18417987269992));
#16050=CARTESIAN_POINT('Ctrl Pts',(6.20912141897563,2.18350559545778,6.18839687576434));
#16051=CARTESIAN_POINT('Ctrl Pts',(6.1359238825023,2.21937098687609,6.19261387882877));
#16052=CARTESIAN_POINT('Ctrl Pts',(6.06115152472833,2.25149590597147,6.19683088189319));
#16053=CARTESIAN_POINT('Ctrl Pts',(5.98606960786345,2.28375382288914,6.20106534343657));
#16054=CARTESIAN_POINT('Ctrl Pts',(5.90940023074128,2.31224003217109,6.20529980497995));
#16055=CARTESIAN_POINT('Ctrl Pts',(5.83155902235822,2.33681448612266,6.20953426652333));
#16056=CARTESIAN_POINT('Ctrl Pts',(5.75392635824854,2.36132310268874,6.21375738352666));
#16057=CARTESIAN_POINT('Ctrl Pts',(5.67512859653218,2.38194081858858,6.21798050053));
#16058=CARTESIAN_POINT('Ctrl Pts',(5.59559036205847,2.39857956601342,6.22220361753333));
#16059=CARTESIAN_POINT('Ctrl Pts',(5.51573163278717,2.41528535832582,6.22644375134673));
#16060=CARTESIAN_POINT('Ctrl Pts',(5.43512691782398,2.4279799835874,6.23068388516014));
#16061=CARTESIAN_POINT('Ctrl Pts',(5.35421146374845,2.43662682042071,6.23492401897354));
#16062=CARTESIAN_POINT('Ctrl Pts',(5.27329600967292,2.44527365725403,6.23916415278694));
#16063=CARTESIAN_POINT('Ctrl Pts',(5.19207028658604,2.44987274134868,6.24340428660035));
#16064=CARTESIAN_POINT('Ctrl Pts',(5.11096794520242,2.4504400509555,6.24764442041375));
#16065=CARTESIAN_POINT('Ctrl Pts',(5.0300194668307,2.45100628429295,6.25187651007271));
#16066=CARTESIAN_POINT('Ctrl Pts',(4.94889190026816,2.44755815532954,6.25610859973168));
#16067=CARTESIAN_POINT('Ctrl Pts',(4.86801616350811,2.44007369682082,6.26034068939064));
#16068=CARTESIAN_POINT('Ctrl Pts',(4.78725601749245,2.43259993539092,6.26456673038268));
#16069=CARTESIAN_POINT('Ctrl Pts',(4.70674744527433,2.42110134449847,6.26879277137472));
#16070=CARTESIAN_POINT('Ctrl Pts',(4.62692183838648,2.40560796367465,6.27301881236676));
#16071=CARTESIAN_POINT('Ctrl Pts',(4.54707427483231,2.39011032127356,6.2772460157649));
#16072=CARTESIAN_POINT('Ctrl Pts',(4.46791051861213,2.37061571435678,6.28147321916303));
#16073=CARTESIAN_POINT('Ctrl Pts',(4.38985766079683,2.34720625437846,6.28570042256116));
#16074=CARTESIAN_POINT('Ctrl Pts',(4.31196589498814,2.32384510879872,6.28991890150388));
#16075=CARTESIAN_POINT('Ctrl Pts',(4.23518089894629,2.29658536317614,6.29413738044661));
#16076=CARTESIAN_POINT('Ctrl Pts',(4.15991560342966,2.26555941502251,6.29835585938933));
#16077=CARTESIAN_POINT('Ctrl Pts',(4.084674989138,2.23454364099232,6.30257295499559));
#16078=CARTESIAN_POINT('Ctrl Pts',(4.01095351499051,2.1997642940384,6.30679005060184));
#16079=CARTESIAN_POINT('Ctrl Pts',(3.9391455109793,2.16140244978007,6.3110071462081));
#16080=CARTESIAN_POINT('Ctrl Pts',(3.86733908275521,2.12304144735128,6.31522414927252));
#16081=CARTESIAN_POINT('Ctrl Pts',(3.79744645050563,2.08109832390347,6.31944115233693));
#16082=CARTESIAN_POINT('Ctrl Pts',(3.72983736708138,2.03580011475037,6.32365815540135));
#16083=CARTESIAN_POINT('Ctrl Pts',(3.66194838066842,1.99031437008456,6.32789261694473));
#16084=CARTESIAN_POINT('Ctrl Pts',(3.59636229036352,1.94144595220464,6.33212707848812));
#16085=CARTESIAN_POINT('Ctrl Pts',(3.53342257406784,1.8894675949568,6.3363615400315));
#16086=CARTESIAN_POINT('Ctrl Pts',(3.4706514794788,1.83762849285379,6.34058465703484));
#16087=CARTESIAN_POINT('Ctrl Pts',(3.410512914677,1.78269643951499,6.34480777403818));
#16088=CARTESIAN_POINT('Ctrl Pts',(3.35331161785923,1.72497997478066,6.34903089104151));
#16089=CARTESIAN_POINT('Ctrl Pts',(3.29587983166521,1.66703094483023,6.35327102485492));
#16090=CARTESIAN_POINT('Ctrl Pts',(3.24140934282751,1.60627537364017,6.35751115866834));
#16091=CARTESIAN_POINT('Ctrl Pts',(3.19016748139282,1.54305868176058,6.36175129248175));
#16092=CARTESIAN_POINT('Ctrl Pts',(3.13892561995814,1.47984198988098,6.36599142629516));
#16093=CARTESIAN_POINT('Ctrl Pts',(3.09091261150799,1.41416459129452,6.37023156010856));
#16094=CARTESIAN_POINT('Ctrl Pts',(3.04635076874625,1.34639915919381,6.37447169392197));
#16095=CARTESIAN_POINT('Ctrl Pts',(3.00187346632249,1.27876228803623,6.37870378358094));
#16096=CARTESIAN_POINT('Ctrl Pts',(2.96066829775085,1.20879296809753,6.3829358732399));
#16097=CARTESIAN_POINT('Ctrl Pts',(2.92298794009431,1.13684095240292,6.38716796289887));
#16098=CARTESIAN_POINT('Ctrl Pts',(2.88536143666844,1.06499177332378,6.39139400389091));
#16099=CARTESIAN_POINT('Ctrl Pts',(2.85124995232441,0.991165934832231,6.39562004488296));
#16100=CARTESIAN_POINT('Ctrl Pts',(2.82086276928559,0.915741857301564,6.399846085875));
#16101=CARTESIAN_POINT('Ctrl Pts',(2.79046722801111,0.840297033780277,6.40407328927313));
#16102=CARTESIAN_POINT('Ctrl Pts',(2.76379827099119,0.763253495899447,6.40830049267127));
#16103=CARTESIAN_POINT('Ctrl Pts',(2.74101913587277,0.685014359702361,6.4125276960694));
#16104=CARTESIAN_POINT('Ctrl Pts',(2.71828701423584,0.606936699968788,6.41674617501212));
#16105=CARTESIAN_POINT('Ctrl Pts',(2.69942882816891,0.527668811345367,6.42096465395484));
#16106=CARTESIAN_POINT('Ctrl Pts',(2.6845579100964,0.447629258849659,6.42518313289756));
#16107=CARTESIAN_POINT('Ctrl Pts',(2.66969186854063,0.367615953167742,6.42940022850382));
#16108=CARTESIAN_POINT('Ctrl Pts',(2.6588105831879,0.286831942657625,6.43361732411008));
#16109=CARTESIAN_POINT('Ctrl Pts',(2.65197641713916,0.205706640134927,6.43783441971634));
#16110=CARTESIAN_POINT('Ctrl Pts',(2.64514240106242,0.124583117862275,6.44205142278076));
#16111=CARTESIAN_POINT('Ctrl Pts',(2.64235536557133,0.0431187816130797,
6.44626842584518));
#16112=CARTESIAN_POINT('Ctrl Pts',(2.64362573752005,-0.0382526019874996,
6.4504854289096));
#16113=CARTESIAN_POINT('Ctrl Pts',(2.64490136883462,-0.119960864780948,
6.45471989045298));
#16114=CARTESIAN_POINT('Ctrl Pts',(2.65026808016464,-0.2015749316877,6.45895435199637));
#16115=CARTESIAN_POINT('Ctrl Pts',(2.65968365842977,-0.282658249302905,
6.46318881353975));
#16116=CARTESIAN_POINT('Ctrl Pts',(2.66907401143223,-0.363524336714368,
6.46741193054308));
#16117=CARTESIAN_POINT('Ctrl Pts',(2.68249144681185,-0.443862060656903,
6.47163504754642));
#16118=CARTESIAN_POINT('Ctrl Pts',(2.6998426393241,-0.523247920716893,6.47585816454975));
#16119=CARTESIAN_POINT('Ctrl Pts',(2.71726374748095,-0.602953661590481,
6.48009829836316));
#16120=CARTESIAN_POINT('Ctrl Pts',(2.73865024951101,-0.681699398717995,
6.48433843217656));
#16121=CARTESIAN_POINT('Ctrl Pts',(2.76385752974272,-0.759072982832983,
6.48857856598997));
#16122=CARTESIAN_POINT('Ctrl Pts',(2.78906480997442,-0.836446566947971,
6.49281869980338));
#16123=CARTESIAN_POINT('Ctrl Pts',(2.8180926435503,-0.912447583674034,6.49705883361678));
#16124=CARTESIAN_POINT('Ctrl Pts',(2.85074906954625,-0.986686855352001,
6.50129896743019));
#16125=CARTESIAN_POINT('Ctrl Pts',(2.88334354152236,-1.06078528426564,6.50553105708915));
#16126=CARTESIAN_POINT('Ctrl Pts',(2.91967443931074,-1.13340509916198,6.5097631467481));
#16127=CARTESIAN_POINT('Ctrl Pts',(2.95958554566773,-1.20414409480789,6.51399523640706));
#16128=CARTESIAN_POINT('Ctrl Pts',(2.99943960952137,-1.27478198753371,6.51822127739911));
#16129=CARTESIAN_POINT('Ctrl Pts',(3.04286349264541,-1.34354399861218,6.52244731839115));
#16130=CARTESIAN_POINT('Ctrl Pts',(3.08965332706221,-1.41004876355144,6.5266733593832));
#16131=CARTESIAN_POINT('Ctrl Pts',(3.13645603139403,-1.47657182115373,6.53090056278133));
#16132=CARTESIAN_POINT('Ctrl Pts',(3.1866263269493,-1.54083597478252,6.53512776617946));
#16133=CARTESIAN_POINT('Ctrl Pts',(3.23991458832602,-1.60248508368977,6.53935496957759));
#16134=CARTESIAN_POINT('Ctrl Pts',(3.29309286893847,-1.66400695601737,6.54357344852031));
#16135=CARTESIAN_POINT('Ctrl Pts',(3.34937597300401,-1.722924199209,6.54779192746304));
#16136=CARTESIAN_POINT('Ctrl Pts',(3.4084741804015,-1.77891416304573,6.55201040640576));
#16137=CARTESIAN_POINT('Ctrl Pts',(3.46755300813493,-1.83488576648309,6.55622750201202));
#16138=CARTESIAN_POINT('Ctrl Pts',(3.5294447688587,-1.88793167753714,6.56044459761829));
#16139=CARTESIAN_POINT('Ctrl Pts',(3.59382293133692,-1.93776613078916,6.56466169322456));
#16140=CARTESIAN_POINT('Ctrl Pts',(3.65819968107186,-1.98759949045158,6.56887869628898));
#16141=CARTESIAN_POINT('Ctrl Pts',(3.72506235591376,-2.03422124889501,6.57309569935341));
#16142=CARTESIAN_POINT('Ctrl Pts',(3.79405253868518,-2.0773868671015,6.57731270241784));
#16143=CARTESIAN_POINT('Ctrl Pts',(3.8633283422246,-2.12073119185039,6.58154716396122));
#16144=CARTESIAN_POINT('Ctrl Pts',(3.93474891393529,-2.16059043725309,6.58578162550459));
#16145=CARTESIAN_POINT('Ctrl Pts',(4.00792488348457,-2.19676273314475,6.59001608704798));
#16146=CARTESIAN_POINT('Ctrl Pts',(4.08090480739528,-2.23283811988862,6.59423920405131));
#16147=CARTESIAN_POINT('Ctrl Pts',(4.15563029003601,-2.26524613902785,6.59846232105464));
#16148=CARTESIAN_POINT('Ctrl Pts',(4.23169513360644,-2.29383491709987,6.60268543805797));
#16149=CARTESIAN_POINT('Ctrl Pts',(4.30806647614328,-2.32253889202919,6.60692557187138));
#16150=CARTESIAN_POINT('Ctrl Pts',(4.38578754448073,-2.34739264670177,6.61116570568478));
#16151=CARTESIAN_POINT('Ctrl Pts',(4.46443378799603,-2.36829352889397,6.61540583949819));
#16152=CARTESIAN_POINT('Ctrl Pts',(4.54308003151132,-2.38919441108616,6.61964597331159));
#16153=CARTESIAN_POINT('Ctrl Pts',(4.6226509801666,-2.40614238428662,6.623886107125));
#16154=CARTESIAN_POINT('Ctrl Pts',(4.70271562875089,-2.41908702275893,6.6281262409384));
#16155=CARTESIAN_POINT('Ctrl Pts',(4.7826283829782,-2.43200710335743,6.63235833059736));
#16156=CARTESIAN_POINT('Ctrl Pts',(4.86333110127249,-2.44098724308891,6.63659042025632));
#16157=CARTESIAN_POINT('Ctrl Pts',(4.94440127321341,-2.44593993297401,6.64082250991527));
#16158=CARTESIAN_POINT('Ctrl Pts',(5.02535557651603,-2.45088554428237,6.64504855090733));
#16159=CARTESIAN_POINT('Ctrl Pts',(5.10667583045455,-2.4518151100593,6.64927459189939));
#16160=CARTESIAN_POINT('Ctrl Pts',(5.18793111540945,-2.44869244592303,6.65350063289144));
#16161=CARTESIAN_POINT('Ctrl Pts',(5.26920875027467,-2.44556892287324,6.65772783628957));
#16162=CARTESIAN_POINT('Ctrl Pts',(5.35042091607628,-2.43839089225638,6.6619550396877));
#16163=CARTESIAN_POINT('Ctrl Pts',(5.43113299206567,-2.42717428764131,6.66618224308583));
#16164=CARTESIAN_POINT('Ctrl Pts',(5.51167848773203,-2.41598083279159,6.67040072202856));
#16165=CARTESIAN_POINT('Ctrl Pts',(5.59172549204208,-2.40076549679264,6.67461920097129));
#16166=CARTESIAN_POINT('Ctrl Pts',(5.67084570003875,-2.38159607179813,6.67883767991402));
#16167=CARTESIAN_POINT('Ctrl Pts',(5.74993996269581,-2.36243293289985,6.68305477552028));
#16168=CARTESIAN_POINT('Ctrl Pts',(5.82810758131926,-2.33931838934439,6.68727187112654));
#16169=CARTESIAN_POINT('Ctrl Pts',(5.90493120065239,-2.31237118081448,6.69148896673281));
#16170=CARTESIAN_POINT('Ctrl Pts',(5.98175313413311,-2.28542456362637,6.69570596979721));
#16171=CARTESIAN_POINT('Ctrl Pts',(6.05723068884913,-2.25464560358251,6.69992297286161));
#16172=CARTESIAN_POINT('Ctrl Pts',(6.13096378062568,-2.22020221392684,6.70413997592601));
#16173=CARTESIAN_POINT('Ctrl Pts',(6.20500212891104,-2.18561622793315,6.7083744374694));
#16174=CARTESIAN_POINT('Ctrl Pts',(6.2772811063499,-2.14733559408313,6.71260889901278));
#16175=CARTESIAN_POINT('Ctrl Pts',(6.34741961762635,-2.10557740033047,6.71684336055617));
#16176=CARTESIAN_POINT('Ctrl Pts',(6.41737022091445,-2.06393108089682,6.7210664775595));
#16177=CARTESIAN_POINT('Ctrl Pts',(6.48519144589907,-2.01882610443071,6.72528959456283));
#16178=CARTESIAN_POINT('Ctrl Pts',(6.55053501525523,-1.97052086037949,6.72951271156617));
#16179=CARTESIAN_POINT('Ctrl Pts',(6.61614188281239,-1.92202097309126,6.73375284537958));
#16180=CARTESIAN_POINT('Ctrl Pts',(6.67925072628806,-1.87029527870239,6.73799297919298));
#16181=CARTESIAN_POINT('Ctrl Pts',(6.73954460630421,-1.81564432694407,6.74223311300639));
#16182=CARTESIAN_POINT('Ctrl Pts',(6.79983848632034,-1.76099337518575,6.7464732468198));
#16183=CARTESIAN_POINT('Ctrl Pts',(6.85731711672737,-1.70341754074068,6.75071338063321));
#16184=CARTESIAN_POINT('Ctrl Pts',(6.9117038862206,-1.64325118035379,6.75495351444662));
#16185=CARTESIAN_POINT('Ctrl Pts',(6.96540918855507,-1.58383870549912,6.7591405193103));
#16186=CARTESIAN_POINT('Ctrl Pts',(7.01630972610998,-1.5216676940111,6.76332752417397));
#16187=CARTESIAN_POINT('Ctrl Pts',(7.06410492824271,-1.45703663236421,6.76751452903765));
#16188=CARTESIAN_POINT('Ctrl Pts',(7.11183727288988,-1.3924905697516,6.77169602739469));
#16189=CARTESIAN_POINT('Ctrl Pts',(7.1564721034002,-1.32549125271769,6.77587752575173));
#16190=CARTESIAN_POINT('Ctrl Pts',(7.19774685860048,-1.256372609025,6.78005902410877));
#16191=CARTESIAN_POINT('Ctrl Pts',(7.23898061525843,-1.18732262143034,6.78423636895026));
#16192=CARTESIAN_POINT('Ctrl Pts',(7.2768606772769,-1.1161578901549,6.78841371379175));
#16193=CARTESIAN_POINT('Ctrl Pts',(7.31116678822483,-1.04324263857445,6.79259105863324));
#16194=CARTESIAN_POINT('Ctrl Pts',(7.34544985857253,-0.97037635818648,6.79676559789491));
#16195=CARTESIAN_POINT('Ctrl Pts',(7.37616354180739,-0.895762320607005,
6.80094013715659));
#16196=CARTESIAN_POINT('Ctrl Pts',(7.40313346544009,-0.819789373348011,
6.80511467641826));
#16197=CARTESIAN_POINT('Ctrl Pts',(7.43010088435272,-0.74382348176215,6.80928882798687));
#16198=CARTESIAN_POINT('Ctrl Pts',(7.45332506264323,-0.666499374327774,
6.81346297955549));
#16199=CARTESIAN_POINT('Ctrl Pts',(7.4726802197878,-0.588224743023826,6.8176371311241));
#16200=CARTESIAN_POINT('Ctrl Pts',(7.4920341913564,-0.509954906334663,6.82181102701027));
#16201=CARTESIAN_POINT('Ctrl Pts',(7.50751950632716,-0.430735124921569,
6.82598492289644));
#16202=CARTESIAN_POINT('Ctrl Pts',(7.51906109382895,-0.350985176538865,
6.83015881878261));
#16203=CARTESIAN_POINT('Ctrl Pts',(7.53061059387715,-0.271180554120406,
6.83433557615944));
#16204=CARTESIAN_POINT('Ctrl Pts',(7.53821091093363,-0.190845511246944,
6.83851233353628));
#16205=CARTESIAN_POINT('Ctrl Pts',(7.54183875718171,-0.110405832283243,
6.84268909091312));
#16206=CARTESIAN_POINT('Ctrl Pts',(7.54353131309225,-0.0728770494291832,
6.84463773892675));
#16207=CARTESIAN_POINT('Ctrl Pts',(7.54435994289274,-0.0353255197729877,
6.84658638694037));
#16208=CARTESIAN_POINT('Ctrl Pts',(7.54432616288253,0.00220558096770259,
6.848535034954));
#16209=CARTESIAN_POINT('',(7.54432706310264,-0.000672762683564314,7.64853503499169));
#16210=CARTESIAN_POINT('Ctrl Pts',(7.5443261628818,0.002205581778286,6.84853503499609));
#16211=CARTESIAN_POINT('Ctrl Pts',(7.54423010976538,0.108924846857743,6.85407599382254));
#16212=CARTESIAN_POINT('Ctrl Pts',(7.53715829815171,0.215335078947657,6.859616952649));
#16213=CARTESIAN_POINT('Ctrl Pts',(7.52325695306015,0.320657306947781,6.86515791147546));
#16214=CARTESIAN_POINT('Ctrl Pts',(7.50935560796859,0.425979534947917,6.87069887030192));
#16215=CARTESIAN_POINT('Ctrl Pts',(7.48862491996705,0.530214102573731,6.87623982912838));
#16216=CARTESIAN_POINT('Ctrl Pts',(7.46126409479691,0.632607768076277,6.88178078795484));
#16217=CARTESIAN_POINT('Ctrl Pts',(7.4403663641171,0.710814299921889,6.8860128776138));
#16218=CARTESIAN_POINT('Ctrl Pts',(7.41555024571081,0.788130093372826,6.89024496727276));
#16219=CARTESIAN_POINT('Ctrl Pts',(7.38690870987745,0.864133806050236,6.89447705693173));
#16220=CARTESIAN_POINT('Ctrl Pts',(7.35830810963956,0.940028891269427,6.89870309792377));
#16221=CARTESIAN_POINT('Ctrl Pts',(7.32589311339101,1.0146151890146,6.90292913891582));
#16222=CARTESIAN_POINT('Ctrl Pts',(7.28980696566916,1.08748467719021,6.90715517990786));
#16223=CARTESIAN_POINT('Ctrl Pts',(7.25371089216619,1.16037420869643,6.91138238330599));
#16224=CARTESIAN_POINT('Ctrl Pts',(7.21394179334606,1.23154554265023,6.91560958670413));
#16225=CARTESIAN_POINT('Ctrl Pts',(7.17069198614259,1.30060859794372,6.91983679010226));
#16226=CARTESIAN_POINT('Ctrl Pts',(7.12753144150325,1.36952911513589,6.92405526904499));
#16227=CARTESIAN_POINT('Ctrl Pts',(7.08090476714711,1.43634964032875,6.92827374798771));
#16228=CARTESIAN_POINT('Ctrl Pts',(7.03104901840722,1.50070706791586,6.93249222693043));
#16229=CARTESIAN_POINT('Ctrl Pts',(6.98120961851626,1.56504339121936,6.9367093225367));
#16230=CARTESIAN_POINT('Ctrl Pts',(6.92814353145589,1.62691785387678,6.94092641814296));
#16231=CARTESIAN_POINT('Ctrl Pts',(6.87212982415079,1.68599818164277,6.94514351374923));
#16232=CARTESIAN_POINT('Ctrl Pts',(6.8161173460357,1.74507721292344,6.94936051681365));
#16233=CARTESIAN_POINT('Ctrl Pts',(6.75715769683468,1.80136189479551,6.95357751987806));
#16234=CARTESIAN_POINT('Ctrl Pts',(6.69556775059093,1.85455582711536,6.95779452294248));
#16235=CARTESIAN_POINT('Ctrl Pts',(6.63372282070967,1.90796998340331,6.96202898448586));
#16236=CARTESIAN_POINT('Ctrl Pts',(6.56922611707195,1.95826742595683,6.96626344602924));
#16237=CARTESIAN_POINT('Ctrl Pts',(6.5024316192481,2.0051891967036,6.97049790757262));
#16238=CARTESIAN_POINT('Ctrl Pts',(6.4358160704707,2.05198525939946,6.97472102457596));
#16239=CARTESIAN_POINT('Ctrl Pts',(6.36691544130852,2.09542350017289,6.9789441415793));
#16240=CARTESIAN_POINT('Ctrl Pts',(6.29610797575115,2.1352918018724,6.98316725858263));
#16241=CARTESIAN_POINT('Ctrl Pts',(6.22501519553358,2.17532075062886,6.98740739239603));
#16242=CARTESIAN_POINT('Ctrl Pts',(6.15200060520609,2.21175072707874,6.99164752620943));
#16243=CARTESIAN_POINT('Ctrl Pts',(6.07746810223493,2.24441545570649,6.99588766002284));
#16244=CARTESIAN_POINT('Ctrl Pts',(6.00293559926375,2.27708018433424,7.00012779383624));
#16245=CARTESIAN_POINT('Ctrl Pts',(5.92688564259963,2.3059795572839,7.00436792764965));
#16246=CARTESIAN_POINT('Ctrl Pts',(5.84973648336748,2.33099792749201,7.00860806146305));
#16247=CARTESIAN_POINT('Ctrl Pts',(5.77273368738217,2.35596883419008,7.01284015112201));
#16248=CARTESIAN_POINT('Ctrl Pts',(5.69434857887908,2.3771666268737,7.01707224078097));
#16249=CARTESIAN_POINT('Ctrl Pts',(5.61498535135583,2.39444030722076,7.02130433043993));
#16250=CARTESIAN_POINT('Ctrl Pts',(5.5357355528398,2.41168929935295,7.02553037143198));
#16251=CARTESIAN_POINT('Ctrl Pts',(5.45551086207915,2.42502522022466,7.02975641242403));
#16252=CARTESIAN_POINT('Ctrl Pts',(5.37473162020512,2.43434651019167,7.03398245341608));
#16253=CARTESIAN_POINT('Ctrl Pts',(5.29393015936008,2.44367036405341,7.03820965681421));
#16254=CARTESIAN_POINT('Ctrl Pts',(5.21257429382933,2.44897725970599,7.04243686021234));
#16255=CARTESIAN_POINT('Ctrl Pts',(5.13109598065973,2.45021657913494,7.04666406361047));
#16256=CARTESIAN_POINT('Ctrl Pts',(5.04978582923756,2.45145334075294,7.0508825425532));
#16257=CARTESIAN_POINT('Ctrl Pts',(4.96835419939216,2.4486392673208,7.05510102149592));
#16258=CARTESIAN_POINT('Ctrl Pts',(4.88723472502729,2.44177595567053,7.05931950043864));
#16259=CARTESIAN_POINT('Ctrl Pts',(4.80614185160747,2.43491489465832,7.0635365960449));
#16260=CARTESIAN_POINT('Ctrl Pts',(4.72536139306116,2.42400727154023,7.06775369165117));
#16261=CARTESIAN_POINT('Ctrl Pts',(4.64532394146655,2.40910670520086,7.07197078725743));
#16262=CARTESIAN_POINT('Ctrl Pts',(4.56528824624983,2.39420646584622,7.07618779032185));
#16263=CARTESIAN_POINT('Ctrl Pts',(4.48599598219533,2.37531354366745,7.08040479338627));
#16264=CARTESIAN_POINT('Ctrl Pts',(4.40786818142601,2.35253279168467,7.08462179645069));
#16265=CARTESIAN_POINT('Ctrl Pts',(4.32941692996306,2.32965772692261,7.08885625799407));
#16266=CARTESIAN_POINT('Ctrl Pts',(4.25214026067395,2.30286269210011,7.09309071953745));
#16267=CARTESIAN_POINT('Ctrl Pts',(4.17644794826881,2.27230403780522,7.09732518108083));
#16268=CARTESIAN_POINT('Ctrl Pts',(4.10095842303284,2.24182725315866,7.10154829808416));
#16269=CARTESIAN_POINT('Ctrl Pts',(4.02704518323414,2.20760722330936,7.1057714150875));
#16270=CARTESIAN_POINT('Ctrl Pts',(3.95509187700223,2.16984612717386,7.10999453209083));
#16271=CARTESIAN_POINT('Ctrl Pts',(3.88284863901015,2.13193287484649,7.11423466590424));
#16272=CARTESIAN_POINT('Ctrl Pts',(3.81258156440701,2.09045020603706,7.11847479971764));
#16273=CARTESIAN_POINT('Ctrl Pts',(3.74464976856326,2.04564675071359,7.12271493353105));
#16274=CARTESIAN_POINT('Ctrl Pts',(3.67671797271953,2.00084329539013,7.12695506734446));
#16275=CARTESIAN_POINT('Ctrl Pts',(3.6111217956416,1.95271938014768,7.13119520115786));
#16276=CARTESIAN_POINT('Ctrl Pts',(3.54818565973068,1.90156320344629,7.13543533497127));
#16277=CARTESIAN_POINT('Ctrl Pts',(3.48536892288112,1.85050407749949,7.13966742463023));
#16278=CARTESIAN_POINT('Ctrl Pts',(3.42496777694522,1.79623370603101,7.14389951428919));
#16279=CARTESIAN_POINT('Ctrl Pts',(3.36732867519254,1.73900927187233,7.14813160394815));
#16280=CARTESIAN_POINT('Ctrl Pts',(3.30977195348277,1.68186662509753,7.1523576449402));
#16281=CARTESIAN_POINT('Ctrl Pts',(3.25496976256563,1.62177862576476,7.15658368593224));
#16282=CARTESIAN_POINT('Ctrl Pts',(3.20323583655671,1.55904288424455,7.16080972692429));
#16283=CARTESIAN_POINT('Ctrl Pts',(3.1514876807212,1.49628988676115,7.16503693032242));
#16284=CARTESIAN_POINT('Ctrl Pts',(3.10280982282825,1.43088800491757,7.16926413372055));
#16285=CARTESIAN_POINT('Ctrl Pts',(3.05747955297212,1.36317228987018,7.17349133711868));
#16286=CARTESIAN_POINT('Ctrl Pts',(3.0122428395127,1.29559633217082,7.17770981606141));
#16287=CARTESIAN_POINT('Ctrl Pts',(2.97034018911735,1.22571645496427,7.18192829500413));
#16288=CARTESIAN_POINT('Ctrl Pts',(2.93200597649514,1.1538974998711,7.18614677394685));
#16289=CARTESIAN_POINT('Ctrl Pts',(2.89368433454466,1.08210209586836,7.19036386955312));
#16290=CARTESIAN_POINT('Ctrl Pts',(2.85892902515503,1.00836928638527,7.19458096515938));
#16291=CARTESIAN_POINT('Ctrl Pts',(2.82792910448836,0.933089638048864,7.19879806076564));
#16292=CARTESIAN_POINT('Ctrl Pts',(2.79692986409792,0.857811641682979,7.20301506383006));
#16293=CARTESIAN_POINT('Ctrl Pts',(2.76968602445695,0.780987304074674,7.20723206689447));
#16294=CARTESIAN_POINT('Ctrl Pts',(2.74633844139469,0.703027017523766,7.21144906995889));
#16295=CARTESIAN_POINT('Ctrl Pts',(2.72289419886087,0.624743973791483,7.21568353150227));
#16296=CARTESIAN_POINT('Ctrl Pts',(2.70337869048469,0.54531600365262,7.21991799304566));
#16297=CARTESIAN_POINT('Ctrl Pts',(2.68788342794357,0.465172043503783,7.22415245458904));
#16298=CARTESIAN_POINT('Ctrl Pts',(2.67242967873883,0.385242796927439,7.22837557159237));
#16299=CARTESIAN_POINT('Ctrl Pts',(2.6609746866025,0.304601860576321,7.23259868859571));
#16300=CARTESIAN_POINT('Ctrl Pts',(2.65355729498283,0.223681152715985,7.23682180559905));
#16301=CARTESIAN_POINT('Ctrl Pts',(2.64611001540496,0.142434379459981,7.24106193941245));
#16302=CARTESIAN_POINT('Ctrl Pts',(2.64273295449464,0.0609060466887959,
7.24530207322586));
#16303=CARTESIAN_POINT('Ctrl Pts',(2.64341263115474,-0.0204672691777702,
7.24954220703926));
#16304=CARTESIAN_POINT('Ctrl Pts',(2.64409230781484,-0.101840585044325,
7.25378234085267));
#16305=CARTESIAN_POINT('Ctrl Pts',(2.64882863273646,-0.183058421088772,
7.25802247466608));
#16306=CARTESIAN_POINT('Ctrl Pts',(2.65755605430675,-0.263691812006185,
7.26226260847948));
#16307=CARTESIAN_POINT('Ctrl Pts',(2.66626691868094,-0.344172229579233,
7.26649469813844));
#16308=CARTESIAN_POINT('Ctrl Pts',(2.67898623277375,-0.424370675316697,
7.2707267877974));
#16309=CARTESIAN_POINT('Ctrl Pts',(2.69568645370932,-0.503856551649172,
7.27495887745637));
#16310=CARTESIAN_POINT('Ctrl Pts',(2.71236280604048,-0.583228823679947,
7.27918491844841));
#16311=CARTESIAN_POINT('Ctrl Pts',(2.73300867017062,-0.661890098062268,
7.28341095944046));
#16312=CARTESIAN_POINT('Ctrl Pts',(2.757544784589,-0.739415264644689,7.2876370004325));
#16313=CARTESIAN_POINT('Ctrl Pts',(2.78208764786022,-0.816961755138957,
7.29186420383064));
#16314=CARTESIAN_POINT('Ctrl Pts',(2.8105228252285,-0.893371052254958,7.29609140722877));
#16315=CARTESIAN_POINT('Ctrl Pts',(2.84271981873416,-0.968228283293825,
7.3003186106269));
#16316=CARTESIAN_POINT('Ctrl Pts',(2.87485036139567,-1.04293101772751,7.30453708956963));
#16317=CARTESIAN_POINT('Ctrl Pts',(2.91072704715064,-1.11608764946923,7.30875556851234));
#16318=CARTESIAN_POINT('Ctrl Pts',(2.95017104523229,-1.18730313362382,7.31297404745507));
#16319=CARTESIAN_POINT('Ctrl Pts',(2.98960210871799,-1.25849526458,7.31719114306133));
#16320=CARTESIAN_POINT('Ctrl Pts',(3.03259793643184,-1.32774710588574,7.32140823866759));
#16321=CARTESIAN_POINT('Ctrl Pts',(3.07893347085764,-1.3946876674644,7.32562533427385));
#16322=CARTESIAN_POINT('Ctrl Pts',(3.12526798847559,-1.4616267600692,7.32984233733827));
#16323=CARTESIAN_POINT('Ctrl Pts',(3.17494180166971,-1.52625429236071,7.33405934040269));
#16324=CARTESIAN_POINT('Ctrl Pts',(3.22768701133766,-1.5882289546916,7.3382763434671));
#16325=CARTESIAN_POINT('Ctrl Pts',(3.28065058725282,-1.65046019339256,7.34251080501048));
#16326=CARTESIAN_POINT('Ctrl Pts',(3.33671074912334,-1.71001618182879,7.34674526655386));
#16327=CARTESIAN_POINT('Ctrl Pts',(3.39555721020248,-1.76658694749463,7.35097972809725));
#16328=CARTESIAN_POINT('Ctrl Pts',(3.45424601580931,-1.8230061545006,7.35520284510058));
#16329=CARTESIAN_POINT('Ctrl Pts',(3.51570583031381,-1.87645583795613,7.35942596210392));
#16330=CARTESIAN_POINT('Ctrl Pts',(3.57959523468405,-1.92666861191125,7.36364907910725));
#16331=CARTESIAN_POINT('Ctrl Pts',(3.64374207778003,-1.97708371538675,7.36788921292066));
#16332=CARTESIAN_POINT('Ctrl Pts',(3.71033774211421,-2.02423550301704,7.37212934673406));
#16333=CARTESIAN_POINT('Ctrl Pts',(3.77900845618769,-2.06789797573816,7.37636948054747));
#16334=CARTESIAN_POINT('Ctrl Pts',(3.84767917026118,-2.11156044845928,7.38060961436088));
#16335=CARTESIAN_POINT('Ctrl Pts',(3.91842449697439,-2.15173342960025,7.38484974817429));
#16336=CARTESIAN_POINT('Ctrl Pts',(3.99084874874287,-2.18823876309943,7.38908988198769));
#16337=CARTESIAN_POINT('Ctrl Pts',(4.06313560110557,-2.22467484063796,7.39332197164666));
#16338=CARTESIAN_POINT('Ctrl Pts',(4.13736469436473,-2.25759312375911,7.39755406130563));
#16339=CARTESIAN_POINT('Ctrl Pts',(4.21315963169929,-2.28678266623772,7.4017861509646));
#16340=CARTESIAN_POINT('Ctrl Pts',(4.28884623996552,-2.3159304898885,7.40601219195665));
#16341=CARTESIAN_POINT('Ctrl Pts',(4.36609381744599,-2.341359991782,7.41023823294871));
#16342=CARTESIAN_POINT('Ctrl Pts',(4.44450245997007,-2.36290661894114,7.41446427394076));
#16343=CARTESIAN_POINT('Ctrl Pts',(4.52293266941293,-2.38445917267091,7.41869147733889));
#16344=CARTESIAN_POINT('Ctrl Pts',(4.60252415455834,-2.4021265292947,7.42291868073702));
#16345=CARTESIAN_POINT('Ctrl Pts',(4.68285775296745,-2.41579270638451,7.42714588413515));
#16346=CARTESIAN_POINT('Ctrl Pts',(4.76302555218719,-2.42943067807672,7.43136436307788));
#16347=CARTESIAN_POINT('Ctrl Pts',(4.843931950515,-2.43908386709375,7.43558284202061));
#16348=CARTESIAN_POINT('Ctrl Pts',(4.92514815533494,-2.44468763749464,7.43980132096334));
#16349=CARTESIAN_POINT('Ctrl Pts',(5.00633772748967,-2.45028957029008,7.44401841656961));
#16350=CARTESIAN_POINT('Ctrl Pts',(5.08783644115445,-2.45184468959133,7.44823551217587));
#16351=CARTESIAN_POINT('Ctrl Pts',(5.16921056632264,-2.44934023593409,7.45245260778214));
#16352=CARTESIAN_POINT('Ctrl Pts',(5.25058290578035,-2.44683583723572,7.45666961084656));
#16353=CARTESIAN_POINT('Ctrl Pts',(5.33183019774403,-2.44027205814725,7.46088661391099));
#16354=CARTESIAN_POINT('Ctrl Pts',(5.41252033682111,-2.42968823229433,7.46510361697541));
#16355=CARTESIAN_POINT('Ctrl Pts',(5.49354453472467,-2.41906058918586,7.46933807851878));
#16356=CARTESIAN_POINT('Ctrl Pts',(5.57400648719473,-2.40437959084619,7.47357254006216));
#16357=CARTESIAN_POINT('Ctrl Pts',(5.65347735077971,-2.38573718352858,7.47780700160553));
#16358=CARTESIAN_POINT('Ctrl Pts',(5.7327353040845,-2.36714472105851,7.48203011860887));
#16359=CARTESIAN_POINT('Ctrl Pts',(5.81100703423499,-2.34461221743159,7.48625323561222));
#16360=CARTESIAN_POINT('Ctrl Pts',(5.88788252019001,-2.31828089922954,7.49047635261556));
#16361=CARTESIAN_POINT('Ctrl Pts',(5.96506777154849,-2.29184348047665,7.49471648642895));
#16362=CARTESIAN_POINT('Ctrl Pts',(6.04084506816645,-2.2615767511839,7.49895662024235));
#16363=CARTESIAN_POINT('Ctrl Pts',(6.11482154119478,-2.22767159031218,7.50319675405574));
#16364=CARTESIAN_POINT('Ctrl Pts',(6.18879801422311,-2.19376642944046,7.50743688786914));
#16365=CARTESIAN_POINT('Ctrl Pts',(6.26097327777291,-2.15622310783739,7.51167702168254));
#16366=CARTESIAN_POINT('Ctrl Pts',(6.33098270718856,-2.11527690641442,7.51591715549593));
#16367=CARTESIAN_POINT('Ctrl Pts',(6.40085931846993,-2.07440838592849,7.52014924515489));
#16368=CARTESIAN_POINT('Ctrl Pts',(6.46883900936586,-2.02999742697252,7.52438133481385));
#16369=CARTESIAN_POINT('Ctrl Pts',(6.53454011865709,-1.98224529452235,7.52861342447282));
#16370=CARTESIAN_POINT('Ctrl Pts',(6.60014732537101,-1.93456141127463,7.53283946546486));
#16371=CARTESIAN_POINT('Ctrl Pts',(6.66348204576312,-1.88354610978607,7.5370655064569));
#16372=CARTESIAN_POINT('Ctrl Pts',(6.72418878096595,-1.82944560456307,7.54129154744894));
#16373=CARTESIAN_POINT('Ctrl Pts',(6.78491221403776,-1.77533021856704,7.54551875084707));
#16374=CARTESIAN_POINT('Ctrl Pts',(6.84300582713173,-1.71812818962213,7.5497459542452));
#16375=CARTESIAN_POINT('Ctrl Pts',(6.89814442098345,-1.65812829880836,7.55397315764334));
#16376=CARTESIAN_POINT('Ctrl Pts',(6.95316921520019,-1.59825224078024,7.55819163658605));
#16377=CARTESIAN_POINT('Ctrl Pts',(7.00525084276425,-1.53559018353007,7.56241011552878));
#16378=CARTESIAN_POINT('Ctrl Pts',(7.0541019676615,-1.47046690225294,7.56662859447149));
#16379=CARTESIAN_POINT('Ctrl Pts',(7.10293707314914,-1.40536497640048,7.57084569007776));
#16380=CARTESIAN_POINT('Ctrl Pts',(7.14854350112565,-1.33780380077239,7.57506278568401));
#16381=CARTESIAN_POINT('Ctrl Pts',(7.19067477458579,-1.26814049384822,7.57927988129027));
#16382=CARTESIAN_POINT('Ctrl Pts',(7.23280512349825,-1.1984787156471,7.58349688435468));
#16383=CARTESIAN_POINT('Ctrl Pts',(7.27146023002579,-1.12671529608906,7.5877138874191));
#16384=CARTESIAN_POINT('Ctrl Pts',(7.30643822496701,-1.05323430682093,7.59193089048351));
#16385=CARTESIAN_POINT('Ctrl Pts',(7.34156102952299,-0.979449104753689,
7.59616535202689));
#16386=CARTESIAN_POINT('Ctrl Pts',(7.37297599659068,-0.903932501601114,
7.60039981357028));
#16387=CARTESIAN_POINT('Ctrl Pts',(7.40052719086937,-0.827094430286303,
7.60463427511366));
#16388=CARTESIAN_POINT('Ctrl Pts',(7.42800457278164,-0.750462215741914,
7.60885739211699));
#16389=CARTESIAN_POINT('Ctrl Pts',(7.45163876205057,-0.672516064085702,
7.61308050912032));
#16390=CARTESIAN_POINT('Ctrl Pts',(7.47132541865873,-0.593676897355996,
7.61730362612365));
#16391=CARTESIAN_POINT('Ctrl Pts',(7.49109140153145,-0.514520052682174,
7.62154375993706));
#16392=CARTESIAN_POINT('Ctrl Pts',(7.50687788911834,-0.434463445243895,
7.62578389375048));
#16393=CARTESIAN_POINT('Ctrl Pts',(7.51863154107007,-0.353940590343589,
7.63002402756389));
#16394=CARTESIAN_POINT('Ctrl Pts',(7.53038519302179,-0.273417735443293,
7.6342641613773));
#16395=CARTESIAN_POINT('Ctrl Pts',(7.53810602691443,-0.192429104207026,
7.63850429519071));
#16396=CARTESIAN_POINT('Ctrl Pts',(7.54179332448113,-0.111408641021635,
7.64274442900412));
#16397=CARTESIAN_POINT('Ctrl Pts',(7.5434718632701,-0.0745263477710347,
7.64467463098741));
#16398=CARTESIAN_POINT('Ctrl Pts',(7.54431692344925,-0.0376058353287276,
7.64660483297071));
#16399=CARTESIAN_POINT('Ctrl Pts',(7.54432706310245,-0.000672763404672779,
7.648535034954));
#16400=CARTESIAN_POINT('',(7.54432655273176,-0.00171870211734679,8.44853500454046));
#16401=CARTESIAN_POINT('Ctrl Pts',(7.54432706310264,-0.000672762683580638,
7.64853503499169));
#16402=CARTESIAN_POINT('Ctrl Pts',(7.54434913504306,0.0797230281083948,
7.65273669238839));
#16403=CARTESIAN_POINT('Ctrl Pts',(7.54041051570088,0.160277450484244,7.65693834978509));
#16404=CARTESIAN_POINT('Ctrl Pts',(7.53249050506243,0.240564580252856,7.6611400071818));
#16405=CARTESIAN_POINT('Ctrl Pts',(7.52458159021615,0.320739229199728,7.66533577813222));
#16406=CARTESIAN_POINT('Ctrl Pts',(7.51270240427672,0.400646863270518,7.66953154908264));
#16407=CARTESIAN_POINT('Ctrl Pts',(7.49688426185791,0.479861223019126,7.67372732003306));
#16408=CARTESIAN_POINT('Ctrl Pts',(7.48108343481771,0.558988870523393,7.67791849806981));
#16409=CARTESIAN_POINT('Ctrl Pts',(7.4613523092814,0.637424290795133,7.68210967610655));
#16410=CARTESIAN_POINT('Ctrl Pts',(7.43777386554785,0.714747556998992,7.6863008541433));
#16411=CARTESIAN_POINT('Ctrl Pts',(7.41420923082455,0.792025537865658,7.69048957756426));
#16412=CARTESIAN_POINT('Ctrl Pts',(7.38680188651039,0.868192206760459,7.69467830098522));
#16413=CARTESIAN_POINT('Ctrl Pts',(7.35568533976967,0.942840285541607,7.69886702440617));
#16414=CARTESIAN_POINT('Ctrl Pts',(7.32457715080152,1.01746831416521,7.70305462275377));
#16415=CARTESIAN_POINT('Ctrl Pts',(7.2897619191421,1.0905781271244,7.70724222110136));
#16416=CARTESIAN_POINT('Ctrl Pts',(7.25142167462184,1.16178145141548,7.71142981944896));
#16417=CARTESIAN_POINT('Ctrl Pts',(7.21307957177601,1.23298822688325,7.7156176207666));
#16418=CARTESIAN_POINT('Ctrl Pts',(7.17121234244202,1.30228791559096,7.71980542208424));
#16419=CARTESIAN_POINT('Ctrl Pts',(7.12604771747699,1.36931728875646,7.72399322340188));
#16420=CARTESIAN_POINT('Ctrl Pts',(7.08083722339248,1.43641473684407,7.72818527784371));
#16421=CARTESIAN_POINT('Ctrl Pts',(7.0323229128709,1.5012368744042,7.73237733228554));
#16422=CARTESIAN_POINT('Ctrl Pts',(6.98077516759307,1.56345049473307,7.73656938672737));
#16423=CARTESIAN_POINT('Ctrl Pts',(6.92919923522218,1.62569813441808,7.74076373344849));
#16424=CARTESIAN_POINT('Ctrl Pts',(6.874586885962,1.68533407022842,7.7449580801696));
#16425=CARTESIAN_POINT('Ctrl Pts',(6.81724628663355,1.7420610633044,7.74915242689072));
#16426=CARTESIAN_POINT('Ctrl Pts',(6.75980868398112,1.79888402166418,7.75335386920516));
#16427=CARTESIAN_POINT('Ctrl Pts',(6.69963396885006,1.85278789834029,7.7575553115196));
#16428=CARTESIAN_POINT('Ctrl Pts',(6.63706398365877,1.90351525921642,7.76175675383404));
#16429=CARTESIAN_POINT('Ctrl Pts',(6.59826927250347,1.93496729339612,7.76436173672682));
#16430=CARTESIAN_POINT('Ctrl Pts',(6.55855437060596,1.96519902747809,7.76696671961959));
#16431=CARTESIAN_POINT('Ctrl Pts',(6.51800593252806,1.99415773220909,7.76957170251236));
#16432=CARTESIAN_POINT('Ctrl Pts',(6.45213040376656,2.04120442689898,7.77380379217132));
#16433=CARTESIAN_POINT('Ctrl Pts',(6.3837982580845,2.08507115137388,7.77803588183027));
#16434=CARTESIAN_POINT('Ctrl Pts',(6.31334926780202,2.12549195893375,7.78226797148922));
#16435=CARTESIAN_POINT('Ctrl Pts',(6.24300096595278,2.16585499550547,7.78649401248125));
#16436=CARTESIAN_POINT('Ctrl Pts',(6.17054222811735,2.20278166749725,7.79072005347329));
#16437=CARTESIAN_POINT('Ctrl Pts',(6.09634314235166,2.236048287943,7.79494609446532));
#16438=CARTESIAN_POINT('Ctrl Pts',(6.02212364753879,2.26932405863662,7.79917329786346));
#16439=CARTESIAN_POINT('Ctrl Pts',(5.94616324199081,2.29893751481314,7.80340050126159));
#16440=CARTESIAN_POINT('Ctrl Pts',(5.86885846271062,2.32471002982538,7.80762770465973));
#16441=CARTESIAN_POINT('Ctrl Pts',(5.79171323149022,2.35042935336868,7.81184618360244));
#16442=CARTESIAN_POINT('Ctrl Pts',(5.71322960321401,2.37232340372805,7.81606466254516));
#16443=CARTESIAN_POINT('Ctrl Pts',(5.63382147252083,2.39026282812886,7.82028314148787));
#16444=CARTESIAN_POINT('Ctrl Pts',(5.55443938158367,2.40819636977899,7.82450023709413));
#16445=CARTESIAN_POINT('Ctrl Pts',(5.47413384320454,2.42217775850298,7.82871733270038));
#16446=CARTESIAN_POINT('Ctrl Pts',(5.39333155283008,2.43212815574177,7.83293442830664));
#16447=CARTESIAN_POINT('Ctrl Pts',(5.31253103561741,2.44207833462457,7.83715143137105));
#16448=CARTESIAN_POINT('Ctrl Pts',(5.23123424942869,2.44799764224542,7.84136843443547));
#16449=CARTESIAN_POINT('Ctrl Pts',(5.14987423854054,2.44985897032409,7.84558543749988));
#16450=CARTESIAN_POINT('Ctrl Pts',(5.0681773955425,2.45172800433909,7.84981989904327));
#16451=CARTESIAN_POINT('Ctrl Pts',(4.98641727461212,2.44950536333508,7.85405436058665));
#16452=CARTESIAN_POINT('Ctrl Pts',(4.90503173006084,2.44321643276869,7.85828882213004));
#16453=CARTESIAN_POINT('Ctrl Pts',(4.82386422540937,2.43694435086748,7.86251193913337));
#16454=CARTESIAN_POINT('Ctrl Pts',(4.74306975124056,2.42662783962624,7.8667350561367));
#16455=CARTESIAN_POINT('Ctrl Pts',(4.66307508507712,2.41234386103366,7.87095817314003));
#16456=CARTESIAN_POINT('Ctrl Pts',(4.58275808495003,2.39800232596067,7.87519830695345));
#16457=CARTESIAN_POINT('Ctrl Pts',(4.50324780944299,2.37966139703988,7.87943844076687));
#16458=CARTESIAN_POINT('Ctrl Pts',(4.42496166673264,2.35744972544458,7.88367857458029));
#16459=CARTESIAN_POINT('Ctrl Pts',(4.34667552402229,2.33523805384928,7.88791870839371));
#16460=CARTESIAN_POINT('Ctrl Pts',(4.26961393682959,2.30915584832735,7.89215884220713));
#16461=CARTESIAN_POINT('Ctrl Pts',(4.19417318033878,2.27937995407983,7.89639897602055));
#16462=CARTESIAN_POINT('Ctrl Pts',(4.11887554600507,2.24966054906191,7.90063106567951));
#16463=CARTESIAN_POINT('Ctrl Pts',(4.04491167209881,2.21615059522029,7.90486315533847));
#16464=CARTESIAN_POINT('Ctrl Pts',(3.97268947649604,2.17899071930625,7.90909524499743));
#16465=CARTESIAN_POINT('Ctrl Pts',(3.90057050366025,2.14188395373011,7.91332128598948));
#16466=CARTESIAN_POINT('Ctrl Pts',(3.83018867490852,2.10113783766115,7.91754732698153));
#16467=CARTESIAN_POINT('Ctrl Pts',(3.76193291616612,2.05694141514875,7.92177336797358));
#16468=CARTESIAN_POINT('Ctrl Pts',(3.69365838313604,2.01273283605988,7.92600057137171));
#16469=CARTESIAN_POINT('Ctrl Pts',(3.62751151362582,1.96507224802607,7.93022777476984));
#16470=CARTESIAN_POINT('Ctrl Pts',(3.56385778900778,1.91419538912277,7.93445497816798));
#16471=CARTESIAN_POINT('Ctrl Pts',(3.50033543826272,1.86342353412991,7.9386734571107));
#16472=CARTESIAN_POINT('Ctrl Pts',(3.43929633018822,1.80944894164393,7.94289193605342));
#16473=CARTESIAN_POINT('Ctrl Pts',(3.38107402306712,1.75254870331811,7.94711041499615));
#16474=CARTESIAN_POINT('Ctrl Pts',(3.32287080838226,1.6956671238917,7.95132751060241));
#16475=CARTESIAN_POINT('Ctrl Pts',(3.26748289235801,1.63586212841871,7.95554460620867));
#16476=CARTESIAN_POINT('Ctrl Pts',(3.21520839209335,1.57344901155158,7.95976170181493));
#16477=CARTESIAN_POINT('Ctrl Pts',(3.16293503896387,1.51103726430599,7.96397870487934));
#16478=CARTESIAN_POINT('Ctrl Pts',(3.11377526324372,1.44601786644287,7.96819570794376));
#16479=CARTESIAN_POINT('Ctrl Pts',(3.06798721296639,1.37873956113017,7.97241271100817));
#16480=CARTESIAN_POINT('Ctrl Pts',(3.02200959922407,1.31118272225693,7.97664717255156));
#16481=CARTESIAN_POINT('Ctrl Pts',(2.97943196451947,1.24134861504183,7.98088163409494));
#16482=CARTESIAN_POINT('Ctrl Pts',(2.94047101054738,1.169618554571,7.98511609563833));
#16483=CARTESIAN_POINT('Ctrl Pts',(2.90161443681309,1.09808066600576,7.98933921264166));
#16484=CARTESIAN_POINT('Ctrl Pts',(2.86635535496317,1.02465740942091,7.99356232964499));
#16485=CARTESIAN_POINT('Ctrl Pts',(2.83486115444528,0.949748838530843,7.99778544664832));
#16486=CARTESIAN_POINT('Ctrl Pts',(2.80324004983536,0.874538427809408,8.00202558046173));
#16487=CARTESIAN_POINT('Ctrl Pts',(2.77541438402111,0.797831153663802,8.00626571427514));
#16488=CARTESIAN_POINT('Ctrl Pts',(2.75150306778021,0.720047302826216,8.01050584808855));
#16489=CARTESIAN_POINT('Ctrl Pts',(2.7275917515393,0.642263451988641,8.01474598190196));
#16490=CARTESIAN_POINT('Ctrl Pts',(2.70759483944073,0.563403492744156,8.01898611571537));
#16491=CARTESIAN_POINT('Ctrl Pts',(2.69157930278514,0.483896171045126,8.02322624952878));
#16492=CARTESIAN_POINT('Ctrl Pts',(2.67559414994663,0.4045396863721,8.02745833918776));
#16493=CARTESIAN_POINT('Ctrl Pts',(2.66351562688301,0.324242233546056,8.03169042884674));
#16494=CARTESIAN_POINT('Ctrl Pts',(2.65544743384357,0.243422643242911,8.03592251850571));
#16495=CARTESIAN_POINT('Ctrl Pts',(2.64739077217901,0.162718563437469,8.04014855949777));
#16496=CARTESIAN_POINT('Ctrl Pts',(2.64333310249604,0.0814942868331558,
8.04437460048982));
#16497=CARTESIAN_POINT('Ctrl Pts',(2.64332716199235,0.000179021789542721,
8.04860064148187));
#16498=CARTESIAN_POINT('Ctrl Pts',(2.64332121985467,-0.0811586096623815,
8.05282784488));
#16499=CARTESIAN_POINT('Ctrl Pts',(2.64736930210422,-0.16258681747649,8.05705504827813));
#16500=CARTESIAN_POINT('Ctrl Pts',(2.65547220897873,-0.243670689669318,
8.06128225167626));
#16501=CARTESIAN_POINT('Ctrl Pts',(2.66355839239734,-0.32458721419525,8.065500730619));
#16502=CARTESIAN_POINT('Ctrl Pts',(2.67568265845143,-0.405160358115837,
8.06971920956173));
#16503=CARTESIAN_POINT('Ctrl Pts',(2.69179374419206,-0.484959525306589,
8.07393768850446));
#16504=CARTESIAN_POINT('Ctrl Pts',(2.7078995467364,-0.564732524511477,8.07815478411074));
#16505=CARTESIAN_POINT('Ctrl Pts',(2.72798948075756,-0.643731595873776,
8.08237187971702));
#16506=CARTESIAN_POINT('Ctrl Pts',(2.75196095221176,-0.721535124658506,
8.0865889753233));
#16507=CARTESIAN_POINT('Ctrl Pts',(2.77593189762514,-0.799336946087373,
8.09080597838772));
#16508=CARTESIAN_POINT('Ctrl Pts',(2.80378407319164,-0.875942833351775,
8.09502298145215));
#16509=CARTESIAN_POINT('Ctrl Pts',(2.83536508321222,-0.950946538060565,
8.09923998451657));
#16510=CARTESIAN_POINT('Ctrl Pts',(2.86707683926029,-1.0262607596411,8.10347444605994));
#16511=CARTESIAN_POINT('Ctrl Pts',(2.90254819921316,-1.09995906444261,8.10770890760331));
#16512=CARTESIAN_POINT('Ctrl Pts',(2.94157689847738,-1.17165228687862,8.11194336914668));
#16513=CARTESIAN_POINT('Ctrl Pts',(2.98050103600779,-1.2431534361023,8.11616648615003));
#16514=CARTESIAN_POINT('Ctrl Pts',(3.02296319737104,-1.31265985532268,8.12038960315338));
#16515=CARTESIAN_POINT('Ctrl Pts',(3.06871858439075,-1.37981358357199,8.12461272015673));
#16516=CARTESIAN_POINT('Ctrl Pts',(3.1146583401429,-1.44723790395399,8.12885285397011));
#16517=CARTESIAN_POINT('Ctrl Pts',(3.16391762583173,-1.51229016262488,8.1330929877835));
#16518=CARTESIAN_POINT('Ctrl Pts',(3.21620830848822,-1.57464209124558,8.13733312159688));
#16519=CARTESIAN_POINT('Ctrl Pts',(3.26849899114471,-1.63699401986627,8.14157325541026));
#16520=CARTESIAN_POINT('Ctrl Pts',(3.32382070737321,-1.69664531808319,8.14581338922364));
#16521=CARTESIAN_POINT('Ctrl Pts',(3.38184999060249,-1.75330671504732,8.15005352303702));
#16522=CARTESIAN_POINT('Ctrl Pts',(3.43976918378828,-1.80986061704842,8.15428561269597));
#16523=CARTESIAN_POINT('Ctrl Pts',(3.50060175364407,-1.86364695448092,8.15851770235492));
#16524=CARTESIAN_POINT('Ctrl Pts',(3.56405252120205,-1.91435101755191,8.16274979201387));
#16525=CARTESIAN_POINT('Ctrl Pts',(3.62741260245876,-1.96498261240673,8.16697583300592));
#16526=CARTESIAN_POINT('Ctrl Pts',(3.69338308935487,-2.01254039464917,8.17120187399797));
#16527=CARTESIAN_POINT('Ctrl Pts',(3.76163238981083,-2.05674678956728,8.17542791499001));
#16528=CARTESIAN_POINT('Ctrl Pts',(3.8299004627781,-2.10096534380487,8.17965511838815));
#16529=CARTESIAN_POINT('Ctrl Pts',(3.90044825105619,-2.14183036022231,8.18388232178627));
#16530=CARTESIAN_POINT('Ctrl Pts',(3.97291114326035,-2.17910475737397,8.18810952518441));
#16531=CARTESIAN_POINT('Ctrl Pts',(4.0452244804956,-2.2163022245117,8.19232800412712));
#16532=CARTESIAN_POINT('Ctrl Pts',(4.11944462263375,-2.24992364401651,8.19654648306983));
#16533=CARTESIAN_POINT('Ctrl Pts',(4.19518228029263,-2.27977798005591,8.20076496201255));
#16534=CARTESIAN_POINT('Ctrl Pts',(4.27089510182833,-2.30962252617058,8.20498205761881));
#16535=CARTESIAN_POINT('Ctrl Pts',(4.34812401865969,-2.33570227176141,8.20919915322506));
#16536=CARTESIAN_POINT('Ctrl Pts',(4.4264593774034,-2.35787414821508,8.21341624883132));
#16537=CARTESIAN_POINT('Ctrl Pts',(4.50479301712052,-2.38004553811905,8.21763325189573));
#16538=CARTESIAN_POINT('Ctrl Pts',(4.5842326030374,-2.3983091039443,8.22185025496013));
#16539=CARTESIAN_POINT('Ctrl Pts',(4.66435430839896,-2.41257193128893,8.22606725802453));
#16540=CARTESIAN_POINT('Ctrl Pts',(4.74480771926037,-2.42689380703065,8.23030171956792));
#16541=CARTESIAN_POINT('Ctrl Pts',(4.82594844733071,-2.43718165208182,8.23453618111131));
#16542=CARTESIAN_POINT('Ctrl Pts',(4.90733989665653,-2.44339369572456,8.2387706426547));
#16543=CARTESIAN_POINT('Ctrl Pts',(4.98851329026299,-2.44958909668977,8.24299375965802));
#16544=CARTESIAN_POINT('Ctrl Pts',(5.06993559493031,-2.4517305361713,8.24721687666135));
#16545=CARTESIAN_POINT('Ctrl Pts',(5.15117328608259,-2.4498289065365,8.25143999366467));
#16546=CARTESIAN_POINT('Ctrl Pts',(5.23273831989722,-2.4479196143931,8.25568012747809));
#16547=CARTESIAN_POINT('Ctrl Pts',(5.31411677973135,-2.44193464489345,8.25992026129152));
#16548=CARTESIAN_POINT('Ctrl Pts',(5.39487650776516,-2.43193740410244,8.26416039510494));
#16549=CARTESIAN_POINT('Ctrl Pts',(5.47563623579896,-2.42194016331143,8.26840052891836));
#16550=CARTESIAN_POINT('Ctrl Pts',(5.55577678239371,-2.40793079298131,8.27264066273178));
#16551=CARTESIAN_POINT('Ctrl Pts',(5.63487951587815,-2.39002355496311,8.2768807965452));
#16552=CARTESIAN_POINT('Ctrl Pts',(5.71383217989905,-2.37215028959648,8.28111288620416));
#16553=CARTESIAN_POINT('Ctrl Pts',(5.79204552480599,-2.35032726670433,8.28534497586312));
#16554=CARTESIAN_POINT('Ctrl Pts',(5.86909494316962,-2.32463117662332,8.28957706552208));
#16555=CARTESIAN_POINT('Ctrl Pts',(5.94603423951164,-2.2989718123924,8.2938031065141));
#16556=CARTESIAN_POINT('Ctrl Pts',(6.02181247612304,-2.26945052093793,8.29802914750613));
#16557=CARTESIAN_POINT('Ctrl Pts',(6.09601642169648,-2.23619474210691,8.30225518849815));
#16558=CARTESIAN_POINT('Ctrl Pts',(6.17024077765402,-2.20292981601,8.30648239189629));
#16559=CARTESIAN_POINT('Ctrl Pts',(6.24288952771448,-2.16592847667754,8.31070959529443));
#16560=CARTESIAN_POINT('Ctrl Pts',(6.31356548021642,-2.12536789029655,8.31493679869257));
#16561=CARTESIAN_POINT('Ctrl Pts',(6.38409556578478,-2.08489101624132,8.31915527763528));
#16562=CARTESIAN_POINT('Ctrl Pts',(6.45266057340652,-2.04086978183839,8.32337375657799));
#16563=CARTESIAN_POINT('Ctrl Pts',(6.51888854564062,-1.99352709642905,8.3275922355207));
#16564=CARTESIAN_POINT('Ctrl Pts',(6.5850948001965,-1.9461999357772,8.33180933112696));
#16565=CARTESIAN_POINT('Ctrl Pts',(6.64896516356059,-1.89555375715765,8.33602642673322));
#16566=CARTESIAN_POINT('Ctrl Pts',(6.71015687043073,-1.84185463663134,8.34024352233948));
#16567=CARTESIAN_POINT('Ctrl Pts',(6.77134723448216,-1.78815669450301,8.34446052540387));
#16568=CARTESIAN_POINT('Ctrl Pts',(6.82985871039997,-1.73140625104065,8.34867752846826));
#16569=CARTESIAN_POINT('Ctrl Pts',(6.88538292579458,-1.67190854168408,8.35289453153265));
#16570=CARTESIAN_POINT('Ctrl Pts',(6.94113701257752,-1.61216451059283,8.35712899307605));
#16571=CARTESIAN_POINT('Ctrl Pts',(6.99387872019512,-1.54965075382522,8.36136345461945));
#16572=CARTESIAN_POINT('Ctrl Pts',(7.04333566297255,-1.48471102545557,8.36559791616285));
#16573=CARTESIAN_POINT('Ctrl Pts',(7.09266010572292,-1.41994527702247,8.36982103316618));
#16574=CARTESIAN_POINT('Ctrl Pts',(7.13871713113803,-1.35276694814826,8.3740441501695));
#16575=CARTESIAN_POINT('Ctrl Pts',(7.18128022620912,-1.28354584156208,8.37826726717283));
#16576=CARTESIAN_POINT('Ctrl Pts',(7.22401482685434,-1.21404581245845,8.38250740098627));
#16577=CARTESIAN_POINT('Ctrl Pts',(7.26322706153285,-1.14248692596317,8.3867475347997));
#16578=CARTESIAN_POINT('Ctrl Pts',(7.29873523791302,-1.06926638304164,8.39098766861314));
#16579=CARTESIAN_POINT('Ctrl Pts',(7.3342434142932,-0.996045840120104,8.39522780242657));
#16580=CARTESIAN_POINT('Ctrl Pts',(7.36604740694082,-0.921164095233479,
8.39946793624001));
#16581=CARTESIAN_POINT('Ctrl Pts',(7.39401556223308,-0.84503464030478,8.40370807005344));
#16582=CARTESIAN_POINT('Ctrl Pts',(7.42616850853488,-0.757514163865443,
8.40858264234436));
#16583=CARTESIAN_POINT('Ctrl Pts',(7.45335219664532,-0.6680757325126,8.41345721463529));
#16584=CARTESIAN_POINT('Ctrl Pts',(7.47536636025846,-0.577253207851724,
8.41833178692621));
#16585=CARTESIAN_POINT('Ctrl Pts',(7.49809992997909,-0.483462672228121,
8.42336565652858));
#16586=CARTESIAN_POINT('Ctrl Pts',(7.5153201250636,-0.388196137854479,8.42839952613096));
#16587=CARTESIAN_POINT('Ctrl Pts',(7.52685978595068,-0.292065864034257,
8.43343339573333));
#16588=CARTESIAN_POINT('Ctrl Pts',(7.53839944683776,-0.195935590214034,
8.43846726533571));
#16589=CARTESIAN_POINT('Ctrl Pts',(7.54425836357543,-0.0989417664283526,
8.44350113493809));
#16590=CARTESIAN_POINT('Ctrl Pts',(7.54432655273176,-0.00171870211734679,
8.44853500454046));
#16591=CARTESIAN_POINT('',(7.54195686003335,0.00183542991444358,9.24853503495399));
#16592=CARTESIAN_POINT('Ctrl Pts',(7.54168864282551,-0.00171626520296555,
8.448535034954));
#16593=CARTESIAN_POINT('Ctrl Pts',(7.5382686113892,0.525630161723889,8.47586847115655));
#16594=CARTESIAN_POINT('Ctrl Pts',(7.11247508906639,1.87364192080501,8.54547766519524));
#16595=CARTESIAN_POINT('Ctrl Pts',(4.89327789020825,2.88797067463353,8.65736261706985));
#16596=CARTESIAN_POINT('Ctrl Pts',(2.56077430391188,1.40151271011197,8.78418989057805));
#16597=CARTESIAN_POINT('Ctrl Pts',(2.54053913495462,-1.36430015381262,8.91101716408634));
#16598=CARTESIAN_POINT('Ctrl Pts',(4.85104382663735,-2.88472717612166,9.03784443759448));
#16599=CARTESIAN_POINT('Ctrl Pts',(7.09724314960541,-1.89752823793867,9.15035039455043));
#16600=CARTESIAN_POINT('Ctrl Pts',(7.53818936996484,-0.537343409699177,
9.22058059367024));
#16601=CARTESIAN_POINT('Ctrl Pts',(7.54195686003335,0.00183542991444358,
9.24853503495399));
#16602=CARTESIAN_POINT('',(7.54821173167671,0.000461678744492038,10.048535034954));
#16603=CARTESIAN_POINT('Ctrl Pts',(7.54195686003335,0.00183542991444358,
9.24853503495399));
#16604=CARTESIAN_POINT('Ctrl Pts',(7.54388697973531,0.278061692569365,9.26285635150631));
#16605=CARTESIAN_POINT('Ctrl Pts',(7.37337365908062,1.36738067873508,9.3194534258947));
#16606=CARTESIAN_POINT('Ctrl Pts',(5.77424895855223,2.81382671743475,9.41832625811913));
#16607=CARTESIAN_POINT('Ctrl Pts',(3.10188641709578,2.10065863938698,9.54515353162742));
#16608=CARTESIAN_POINT('Ctrl Pts',(2.24784426931667,-0.530071728273779,
9.67198080513556));
#16609=CARTESIAN_POINT('Ctrl Pts',(3.99172515361836,-2.67693216321298,9.79880807864387));
#16610=CARTESIAN_POINT('Ctrl Pts',(6.71326072902087,-2.38324880778346,9.92432615524993));
#16611=CARTESIAN_POINT('Ctrl Pts',(7.54617390178795,-0.784506859752817,
10.00756847402));
#16612=CARTESIAN_POINT('Ctrl Pts',(7.54821173167671,0.000461678744492038,
10.048535034954));
#16613=CARTESIAN_POINT('',(7.54432619404612,-0.00217068071248294,10.848535034954));
#16614=CARTESIAN_POINT('Ctrl Pts',(7.54821173167671,0.000461678744492038,
10.048535034954));
#16615=CARTESIAN_POINT('Ctrl Pts',(7.54827685602488,0.0255474646978529,
10.0498442318561));
#16616=CARTESIAN_POINT('Ctrl Pts',(7.54792542615634,0.0506313813797534,
10.0511534287582));
#16617=CARTESIAN_POINT('Ctrl Pts',(7.52217079946011,0.885275564505149,10.0947383834963));
#16618=CARTESIAN_POINT('Ctrl Pts',(6.59176120172026,2.47725417354276,10.1792898991685));
#16619=CARTESIAN_POINT('Ctrl Pts',(3.82877479129759,2.60388883938323,10.3061171726766));
#16620=CARTESIAN_POINT('Ctrl Pts',(2.22057700338537,0.353593297184827,10.4329444461849));
#16621=CARTESIAN_POINT('Ctrl Pts',(3.23519287125426,-2.21947591850572,10.559771719693));
#16622=CARTESIAN_POINT('Ctrl Pts',(5.94644183489036,-2.76652172461777,10.6865989932015));
#16623=CARTESIAN_POINT('Ctrl Pts',(7.41343416718733,-1.26507931657609,10.7828532647379));
#16624=CARTESIAN_POINT('Ctrl Pts',(7.54521040552383,-0.227592870575658,
10.8368317784384));
#16625=CARTESIAN_POINT('Ctrl Pts',(7.54327304612934,-0.00217939107654637,
10.8485345343029));
#16626=CARTESIAN_POINT('',(7.5443269150918,0.00108536201693948,11.6485350350021));
#16627=CARTESIAN_POINT('Ctrl Pts',(7.54432619404612,-0.00217068071248294,
10.848535034954));
#16628=CARTESIAN_POINT('Ctrl Pts',(7.54439758870431,0.0784273272084078,
10.8527176653695));
#16629=CARTESIAN_POINT('Ctrl Pts',(7.54048835863867,0.159110489711957,10.8569002957851));
#16630=CARTESIAN_POINT('Ctrl Pts',(7.53260002673345,0.239451732729212,10.8610829262006));
#16631=CARTESIAN_POINT('Ctrl Pts',(7.52471552024031,0.319754014611907,10.8652635282678));
#16632=CARTESIAN_POINT('Ctrl Pts',(7.51285578733571,0.399714235407546,10.869444130335));
#16633=CARTESIAN_POINT('Ctrl Pts',(7.49707436666984,0.478908228973995,10.8736247324022));
#16634=CARTESIAN_POINT('Ctrl Pts',(7.48129555878778,0.558089111123662,10.8778046423258));
#16635=CARTESIAN_POINT('Ctrl Pts',(7.46159644552335,0.636503553587562,10.8819845522494));
#16636=CARTESIAN_POINT('Ctrl Pts',(7.43808179808031,0.713736940700719,10.886164462173));
#16637=CARTESIAN_POINT('Ctrl Pts',(7.41456353342076,0.790982208488829,10.8903450150847));
#16638=CARTESIAN_POINT('Ctrl Pts',(7.38722870974025,0.867045607888982,10.8945255679965));
#16639=CARTESIAN_POINT('Ctrl Pts',(7.35623167927006,0.941528555388835,10.8987061209082));
#16640=CARTESIAN_POINT('Ctrl Pts',(7.3252008460254,1.01609272777502,10.902891232782));
#16641=CARTESIAN_POINT('Ctrl Pts',(7.29050002116863,1.08907257212126,10.9070763446559));
#16642=CARTESIAN_POINT('Ctrl Pts',(7.2523310345847,1.16009105408751,10.9112614565297));
#16643=CARTESIAN_POINT('Ctrl Pts',(7.21413743490858,1.23115533198916,10.9154492671533));
#16644=CARTESIAN_POINT('Ctrl Pts',(7.17247147012247,1.30025532719584,10.919637077777));
#16645=CARTESIAN_POINT('Ctrl Pts',(7.12757877001081,1.36704228913517,10.9238248884006));
#16646=CARTESIAN_POINT('Ctrl Pts',(7.08261342784854,1.43393732080205,10.92801947543));
#16647=CARTESIAN_POINT('Ctrl Pts',(7.03441121891333,1.4985114758326,10.9322140624593));
#16648=CARTESIAN_POINT('Ctrl Pts',(6.98325807194982,1.56044899365099,10.9364086494887));
#16649=CARTESIAN_POINT('Ctrl Pts',(6.9676285428175,1.57937362090447,10.9376902797317));
#16650=CARTESIAN_POINT('Ctrl Pts',(6.95172377932987,1.59805236370055,10.9389719099747));
#16651=CARTESIAN_POINT('Ctrl Pts',(6.93555258950466,1.61647693319998,10.9402535402177));
#16652=CARTESIAN_POINT('Ctrl Pts',(6.88215346157301,1.67731697987681,10.9444856306234));
#16653=CARTESIAN_POINT('Ctrl Pts',(6.82563677562139,1.73562167331044,10.9487177210291));
#16654=CARTESIAN_POINT('Ctrl Pts',(6.76627263775363,1.79105453817927,10.9529498114348));
#16655=CARTESIAN_POINT('Ctrl Pts',(6.7069933456937,1.84640817598664,10.9571758531528));
#16656=CARTESIAN_POINT('Ctrl Pts',(6.64487502138773,1.89889782280003,10.9614018948708));
#16657=CARTESIAN_POINT('Ctrl Pts',(6.5802269316755,1.94822122851745,10.9656279365888));
#16658=CARTESIAN_POINT('Ctrl Pts',(6.5155610739181,1.99755819040497,10.9698551398029));
#16659=CARTESIAN_POINT('Ctrl Pts',(6.44836438740582,2.04372683777131,10.9740823430169));
#16660=CARTESIAN_POINT('Ctrl Pts',(6.37898217395731,2.08646275509856,10.978309546231));
#16661=CARTESIAN_POINT('Ctrl Pts',(6.30974314328738,2.12911047911107,10.9825280258447));
#16662=CARTESIAN_POINT('Ctrl Pts',(6.23832797970495,2.16833936204999,10.9867465054583));
#16663=CARTESIAN_POINT('Ctrl Pts',(6.16511013076783,2.20392899994552,10.990964985072));
#16664=CARTESIAN_POINT('Ctrl Pts',(6.09191629202919,2.23950696699463,10.9951820813272));
#16665=CARTESIAN_POINT('Ctrl Pts',(6.01692135951698,2.27144785601566,10.9993991775824));
#16666=CARTESIAN_POINT('Ctrl Pts',(5.94052277285337,2.29957752238866,11.0036162738377));
#16667=CARTESIAN_POINT('Ctrl Pts',(5.86412586312688,2.32770657131986,11.0078332775283));
#16668=CARTESIAN_POINT('Ctrl Pts',(5.78632579697358,2.35202440445222,11.0120502812188));
#16669=CARTESIAN_POINT('Ctrl Pts',(5.70753800194581,2.37240579305,11.0162672849094));
#16670=CARTESIAN_POINT('Ctrl Pts',(5.62842405069097,2.39287155406619,11.0205017456442));
#16671=CARTESIAN_POINT('Ctrl Pts',(5.54831462892302,2.40936807926501,11.0247362063789));
#16672=CARTESIAN_POINT('Ctrl Pts',(5.46764182776139,2.42182015037596,11.0289706671136));
#16673=CARTESIAN_POINT('Ctrl Pts',(5.38718513086499,2.43423886519286,11.0331937846817));
#16674=CARTESIAN_POINT('Ctrl Pts',(5.30616853838209,2.44263475937085,11.0374169022497));
#16675=CARTESIAN_POINT('Ctrl Pts',(5.22502512901692,2.44698535789096,11.0416400198178));
#16676=CARTESIAN_POINT('Ctrl Pts',(5.14355479652035,2.45135348477601,11.0458801521358));
#16677=CARTESIAN_POINT('Ctrl Pts',(5.06195709457966,2.45164365752031,11.0501202844539));
#16678=CARTESIAN_POINT('Ctrl Pts',(4.98066777652221,2.44788586436541,11.0543604167719));
#16679=CARTESIAN_POINT('Ctrl Pts',(4.89937845846479,2.4441280712105,11.0586005490899));
#16680=CARTESIAN_POINT('Ctrl Pts',(4.81839798349671,2.4363224189142,11.0628406814079));
#16681=CARTESIAN_POINT('Ctrl Pts',(4.73815252935017,2.42455064091195,11.067080813726));
#16682=CARTESIAN_POINT('Ctrl Pts',(4.65805914449168,2.41280117103816,11.0713129107738));
#16683=CARTESIAN_POINT('Ctrl Pts',(4.57839918700369,2.39705677527953,11.0755450078217));
#16684=CARTESIAN_POINT('Ctrl Pts',(4.49960190535111,2.3773612687476,11.0797771048696));
#16685=CARTESIAN_POINT('Ctrl Pts',(4.42091724289576,2.35769391156408,11.0840031532903));
#16686=CARTESIAN_POINT('Ctrl Pts',(4.34309325453466,2.33408677097203,11.0882292017111));
#16687=CARTESIAN_POINT('Ctrl Pts',(4.26655174843519,2.30663513606798,11.0924552501319));
#16688=CARTESIAN_POINT('Ctrl Pts',(4.18998935711926,2.27917601067456,11.0966824516778));
#16689=CARTESIAN_POINT('Ctrl Pts',(4.11471060530473,2.24787038661509,11.1009096532237));
#16690=CARTESIAN_POINT('Ctrl Pts',(4.04112512980976,2.21286436439434,11.1051368547697));
#16691=CARTESIAN_POINT('Ctrl Pts',(3.96769136394277,2.17793051335374,11.109355341183));
#16692=CARTESIAN_POINT('Ctrl Pts',(3.89594432977266,2.1393116840397,11.1135738275964));
#16693=CARTESIAN_POINT('Ctrl Pts',(3.82627202458665,2.09720152589447,11.1177923140098));
#16694=CARTESIAN_POINT('Ctrl Pts',(3.75662256652938,2.05510517662499,11.1220094170858));
#16695=CARTESIAN_POINT('Ctrl Pts',(3.68904688372532,2.00952001234369,11.1262265201618));
#16696=CARTESIAN_POINT('Ctrl Pts',(3.62390718692327,1.9606849660558,11.1304436232378));
#16697=CARTESIAN_POINT('Ctrl Pts',(3.55876891974422,1.91185099155222,11.1346606337609));
#16698=CARTESIAN_POINT('Ctrl Pts',(3.49606690338341,1.8597675565151,11.138877644284));
#16699=CARTESIAN_POINT('Ctrl Pts',(3.43613206856243,1.80471528194851,11.1430946548071));
#16700=CARTESIAN_POINT('Ctrl Pts',(3.37594933440138,1.74943530303311,11.1473291075094));
#16701=CARTESIAN_POINT('Ctrl Pts',(3.31855707759335,1.69116218289615,11.1515635602116));
#16702=CARTESIAN_POINT('Ctrl Pts',(3.26425330714429,1.63021771048669,11.1557980129139));
#16703=CARTESIAN_POINT('Ctrl Pts',(3.21009481444188,1.56943628155559,11.160021137273));
#16704=CARTESIAN_POINT('Ctrl Pts',(3.15900856526425,1.50599816532624,11.1642442616321));
#16705=CARTESIAN_POINT('Ctrl Pts',(3.11124883825198,1.4402546532346,11.1684673859912));
#16706=CARTESIAN_POINT('Ctrl Pts',(3.06329694122607,1.37424661007452,11.172707502865));
#16707=CARTESIAN_POINT('Ctrl Pts',(3.01869864295373,1.30591497909931,11.1769476197388));
#16708=CARTESIAN_POINT('Ctrl Pts',(2.97766563737836,1.23564180870493,11.1811877366127));
#16709=CARTESIAN_POINT('Ctrl Pts',(2.93663263180299,1.16536863831054,11.1854278534865));
#16710=CARTESIAN_POINT('Ctrl Pts',(2.89916507892861,1.09315437195268,11.1896679703603));
#16711=CARTESIAN_POINT('Ctrl Pts',(2.86542603596681,1.01940114806303,11.1939080872342));
#16712=CARTESIAN_POINT('Ctrl Pts',(2.83175100969359,0.945787864039777,11.1981401588816));
#16713=CARTESIAN_POINT('Ctrl Pts',(2.80166470758439,0.870366826279314,11.2023722305289));
#16714=CARTESIAN_POINT('Ctrl Pts',(2.77536368487898,0.793522139334085,11.2066043021763));
#16715=CARTESIAN_POINT('Ctrl Pts',(2.74910025282121,0.71678728239748,11.2108303251496));
#16716=CARTESIAN_POINT('Ctrl Pts',(2.72661150434788,0.638633253481783,11.2150563481229));
#16717=CARTESIAN_POINT('Ctrl Pts',(2.70804674541415,0.559465892681889,11.2192823710962));
#16718=CARTESIAN_POINT('Ctrl Pts',(2.68947678113385,0.480276334257343,11.2235095789981));
#16719=CARTESIAN_POINT('Ctrl Pts',(2.67483317695073,0.400073310493394,11.2277367869));
#16720=CARTESIAN_POINT('Ctrl Pts',(2.66421597596828,0.319280075360713,11.231963994802));
#16721=CARTESIAN_POINT('Ctrl Pts',(2.65362074391374,0.238654016187215,11.2361824558387));
#16722=CARTESIAN_POINT('Ctrl Pts',(2.64703535431247,0.157440643226408,11.2404009168754));
#16723=CARTESIAN_POINT('Ctrl Pts',(2.64450817448571,0.0760708845275549,
11.2446193779122));
#16724=CARTESIAN_POINT('Ctrl Pts',(2.64198182333396,-0.00527219261689159,
11.2488364556943));
#16725=CARTESIAN_POINT('Ctrl Pts',(2.64351105370798,-0.0867710895524872,
11.2530535334763));
#16726=CARTESIAN_POINT('Ctrl Pts',(2.64909220679532,-0.167991906981183,
11.2572706112584));
#16727=CARTESIAN_POINT('Ctrl Pts',(2.65467323754636,-0.249210944087131,
11.2614875966041));
#16728=CARTESIAN_POINT('Ctrl Pts',(2.66430598141719,-0.330151450284385,
11.2657045819498));
#16729=CARTESIAN_POINT('Ctrl Pts',(2.67793478526406,-0.41038312058654,11.2699215672955));
#16730=CARTESIAN_POINT('Ctrl Pts',(2.69162013879732,-0.490947694336733,
11.2741560500827));
#16731=CARTESIAN_POINT('Ctrl Pts',(2.70933471837483,-0.570797069989575,
11.27839053287));
#16732=CARTESIAN_POINT('Ctrl Pts',(2.73097041610576,-0.649506181125932,
11.2826250156572));
#16733=CARTESIAN_POINT('Ctrl Pts',(2.75254795311202,-0.728003707732052,
11.2868481153779));
#16734=CARTESIAN_POINT('Ctrl Pts',(2.77802536847771,-0.805366661228117,
11.2910712150986));
#16735=CARTESIAN_POINT('Ctrl Pts',(2.80724602416878,-0.881190660444427,
11.2952943148192));
#16736=CARTESIAN_POINT('Ctrl Pts',(2.83658482317548,-0.957321227000153,
11.2995344891398));
#16737=CARTESIAN_POINT('Ctrl Pts',(2.86969699642403,-1.03189994103223,11.3037746634603));
#16738=CARTESIAN_POINT('Ctrl Pts',(2.90637692938527,-1.10454142451776,11.3080148377808));
#16739=CARTESIAN_POINT('Ctrl Pts',(2.94305686234651,-1.17718290800332,11.3122550121013));
#16740=CARTESIAN_POINT('Ctrl Pts',(2.98330426974135,-1.24788678555084,11.3164951864219));
#16741=CARTESIAN_POINT('Ctrl Pts',(3.02687023336538,-1.31629758498359,11.3207353607424));
#16742=CARTESIAN_POINT('Ctrl Pts',(3.07035323835108,-1.38457811605323,11.3249674608908));
#16743=CARTESIAN_POINT('Ctrl Pts',(3.11730439207376,-1.45082905390806,11.3291995610392));
#16744=CARTESIAN_POINT('Ctrl Pts',(3.16750813329105,-1.51467662385626,11.3334316611877));
#16745=CARTESIAN_POINT('Ctrl Pts',(3.21764012001026,-1.5784329386465,11.3376577125394));
#16746=CARTESIAN_POINT('Ctrl Pts',(3.27101517634973,-1.63979234568297,11.3418837638912));
#16747=CARTESIAN_POINT('Ctrl Pts',(3.3273738135302,-1.69840891448714,11.346109815243));
#16748=CARTESIAN_POINT('Ctrl Pts',(3.38374777964987,-1.75704142636348,11.350337016035));
#16749=CARTESIAN_POINT('Ctrl Pts',(3.44310667705206,-1.81292922893659,11.3545642168269));
#16750=CARTESIAN_POINT('Ctrl Pts',(3.50514962997472,-1.86575828285442,11.3587914176189));
#16751=CARTESIAN_POINT('Ctrl Pts',(3.5670647180324,-1.9184784609124,11.3630099065358));
#16752=CARTESIAN_POINT('Ctrl Pts',(3.6316524718586,-1.96815216501466,11.3672283954526));
#16753=CARTESIAN_POINT('Ctrl Pts',(3.69857747712651,-2.01450455078402,11.3714468843695));
#16754=CARTESIAN_POINT('Ctrl Pts',(3.76548053355875,-2.06084173474809,11.3756639897837));
#16755=CARTESIAN_POINT('Ctrl Pts',(3.83471893746229,-2.10385949918518,11.379881095198));
#16756=CARTESIAN_POINT('Ctrl Pts',(3.90592650012927,-2.14332505306153,11.3840982006122));
#16757=CARTESIAN_POINT('Ctrl Pts',(3.9771324971775,-2.18278973922089,11.3883152133063));
#16758=CARTESIAN_POINT('Ctrl Pts',(4.05030715991266,-2.21870214584994,11.3925322260003));
#16759=CARTESIAN_POINT('Ctrl Pts',(4.12505905329797,-2.25087507744138,11.3967492386944));
#16760=CARTESIAN_POINT('Ctrl Pts',(4.20012003846211,-2.28318104096292,11.4009836883241));
#16761=CARTESIAN_POINT('Ctrl Pts',(4.27677089713528,-2.31171634061407,11.4052181379537));
#16762=CARTESIAN_POINT('Ctrl Pts',(4.35459609551625,-2.33634066223756,11.4094525875834));
#16763=CARTESIAN_POINT('Ctrl Pts',(4.43221317814195,-2.36089913488925,11.4136757136868));
#16764=CARTESIAN_POINT('Ctrl Pts',(4.51099786507144,-2.38156744102214,11.4178988397902));
#16765=CARTESIAN_POINT('Ctrl Pts',(4.59052558684527,-2.39825723829553,11.4221219658935));
#16766=CARTESIAN_POINT('Ctrl Pts',(4.6703731667867,-2.4150141614447,11.4263620772864));
#16767=CARTESIAN_POINT('Ctrl Pts',(4.75096930409871,-2.42776044033142,11.4306021886792));
#16768=CARTESIAN_POINT('Ctrl Pts',(4.83187878393395,-2.43645917278711,11.4348423000721));
#16769=CARTESIAN_POINT('Ctrl Pts',(4.91278826376918,-2.44515790524281,11.439082411465));
#16770=CARTESIAN_POINT('Ctrl Pts',(4.99401061602312,-2.4498091266491,11.4433225228578));
#16771=CARTESIAN_POINT('Ctrl Pts',(5.0751121874727,-2.45042853394534,11.4475626342507));
#16772=CARTESIAN_POINT('Ctrl Pts',(5.1560611600733,-2.45104677577907,11.4517947675476));
#16773=CARTESIAN_POINT('Ctrl Pts',(5.2371917788119,-2.44765068432874,11.4560269008445));
#16774=CARTESIAN_POINT('Ctrl Pts',(5.31807313171866,-2.44021802143348,11.4602590341414));
#16775=CARTESIAN_POINT('Ctrl Pts',(5.39883889267889,-2.43279598096157,11.4644851190661));
#16776=CARTESIAN_POINT('Ctrl Pts',(5.47935563647557,-2.42134886884991,11.4687112039909));
#16777=CARTESIAN_POINT('Ctrl Pts',(5.55919194504468,-2.40590645342008,11.4729372889156));
#16778=CARTESIAN_POINT('Ctrl Pts',(5.63904917625865,-2.39045999100737,11.4771644813674));
#16779=CARTESIAN_POINT('Ctrl Pts',(5.71822514934162,-2.37101615404332,11.4813916738192));
#16780=CARTESIAN_POINT('Ctrl Pts',(5.79629273058369,-2.3476567819331,11.485618866271));
#16781=CARTESIAN_POINT('Ctrl Pts',(5.87420020970802,-2.32434531555896,11.4898373895357));
#16782=CARTESIAN_POINT('Ctrl Pts',(5.9510033863069,-2.29713446733452,11.4940559128005));
#16783=CARTESIAN_POINT('Ctrl Pts',(6.0262892383907,-2.2661563745434,11.4982744360653));
#16784=CARTESIAN_POINT('Ctrl Pts',(6.10155040361138,-2.23518843972905,11.5024915760408));
#16785=CARTESIAN_POINT('Ctrl Pts',(6.17529480300427,-2.20045589024738,11.5067087160164));
#16786=CARTESIAN_POINT('Ctrl Pts',(6.24712798438816,-2.16213955330772,11.5109258559919));
#16787=CARTESIAN_POINT('Ctrl Pts',(6.31895958922144,-2.12382405731154,11.5151429034123));
#16788=CARTESIAN_POINT('Ctrl Pts',(6.38887964998971,-2.08192514995343,11.5193599508327));
#16789=CARTESIAN_POINT('Ctrl Pts',(6.45651826229098,-2.03666963382503,11.523576998253));
#16790=CARTESIAN_POINT('Ctrl Pts',(6.52443534469827,-1.99122779943927,11.5278114073785));
#16791=CARTESIAN_POINT('Ctrl Pts',(6.59005175412252,-1.9424019110021,11.532045816504));
#16792=CARTESIAN_POINT('Ctrl Pts',(6.6530238549092,-1.89046446737442,11.5362802256295));
#16793=CARTESIAN_POINT('Ctrl Pts',(6.71582867708937,-1.83866498997443,11.540503386503));
#16794=CARTESIAN_POINT('Ctrl Pts',(6.77600290369533,-1.78377081286643,11.5447265473765));
#16795=CARTESIAN_POINT('Ctrl Pts',(6.83324159173854,-1.72609028409346,11.54894970825));
#16796=CARTESIAN_POINT('Ctrl Pts',(6.89070895986495,-1.66817930999461,11.5531897415015));
#16797=CARTESIAN_POINT('Ctrl Pts',(6.94521697590909,-1.60746003023737,11.5574297747529));
#16798=CARTESIAN_POINT('Ctrl Pts',(6.99649810758367,-1.54427766218338,11.5616698080044));
#16799=CARTESIAN_POINT('Ctrl Pts',(7.04777923925826,-1.4810952941294,11.5659098412559));
#16800=CARTESIAN_POINT('Ctrl Pts',(7.0958332607517,-1.41545025153213,11.5701498745074));
#16801=CARTESIAN_POINT('Ctrl Pts',(7.14043763303792,-1.34771503035326,11.5743899077589));
#16802=CARTESIAN_POINT('Ctrl Pts',(7.18580626072282,-1.27881922769294,11.5787025901283));
#16803=CARTESIAN_POINT('Ctrl Pts',(7.22777065521348,-1.20751132097549,11.5830152724977));
#16804=CARTESIAN_POINT('Ctrl Pts',(7.26607126061476,-1.13415422125497,11.5873279548672));
#16805=CARTESIAN_POINT('Ctrl Pts',(7.30431097491278,-1.06091374618534,11.591633780844));
#16806=CARTESIAN_POINT('Ctrl Pts',(7.33889827398536,-0.985630940696496,
11.5959396068208));
#16807=CARTESIAN_POINT('Ctrl Pts',(7.36961701700286,-0.908697285165616,
11.6002454327976));
#16808=CARTESIAN_POINT('Ctrl Pts',(7.40028604158352,-0.831888147135061,
11.6045442897739));
#16809=CARTESIAN_POINT('Ctrl Pts',(7.42709880731689,-0.753433883498876,
11.6088431467502));
#16810=CARTESIAN_POINT('Ctrl Pts',(7.44988590611216,-0.673748776208844,
11.6131420037265));
#16811=CARTESIAN_POINT('Ctrl Pts',(7.47265125111263,-0.59413974062448,11.6174367567818));
#16812=CARTESIAN_POINT('Ctrl Pts',(7.49139844590941,-0.513302618978107,
11.6217315098371));
#16813=CARTESIAN_POINT('Ctrl Pts',(7.50600706647091,-0.431669233189206,
11.6260262628924));
#16814=CARTESIAN_POINT('Ctrl Pts',(7.52060499333906,-0.350095604061897,
11.6303178721347));
#16815=CARTESIAN_POINT('Ctrl Pts',(7.53107029247444,-0.267727303234328,
11.6346094813769));
#16816=CARTESIAN_POINT('Ctrl Pts',(7.53733332939813,-0.185007642795082,
11.6389010906192));
#16817=CARTESIAN_POINT('Ctrl Pts',(7.54201981921922,-0.123110379314718,
11.6421124053974));
#16818=CARTESIAN_POINT('Ctrl Pts',(7.54435442096618,-0.0610166788267173,
11.6453237201757));
#16819=CARTESIAN_POINT('Ctrl Pts',(7.54432691509222,0.00108536108698895,
11.648535034954));
#16820=CARTESIAN_POINT('',(7.54432661325899,0.0016301205695403,12.448535034954));
#16821=CARTESIAN_POINT('Ctrl Pts',(7.5443269150918,0.00108536201690472,
11.6485350350021));
#16822=CARTESIAN_POINT('Ctrl Pts',(7.54428737102145,0.0903668490952409,
11.653151807));
#16823=CARTESIAN_POINT('Ctrl Pts',(7.53936432127917,0.179489947527524,11.6577685789978));
#16824=CARTESIAN_POINT('Ctrl Pts',(7.52963449152874,0.26794191818403,11.6623853509957));
#16825=CARTESIAN_POINT('Ctrl Pts',(7.51987558796534,0.356658193162158,11.6670159184216));
#16826=CARTESIAN_POINT('Ctrl Pts',(7.50528126174495,0.444699028238786,11.6716464858474));
#16827=CARTESIAN_POINT('Ctrl Pts',(7.48597916961371,0.53156278194337,11.6762770532733));
#16828=CARTESIAN_POINT('Ctrl Pts',(7.466590452723,0.61881636653884,11.6809284019588));
#16829=CARTESIAN_POINT('Ctrl Pts',(7.44245175505355,0.704881992755861,11.6855797506444));
#16830=CARTESIAN_POINT('Ctrl Pts',(7.41374112037227,0.789271464942855,11.69023109933));
#16831=CARTESIAN_POINT('Ctrl Pts',(7.39113711119857,0.855711668186527,11.6938931266423));
#16832=CARTESIAN_POINT('Ctrl Pts',(7.36570018578957,0.921113268291848,11.6975551539547));
#16833=CARTESIAN_POINT('Ctrl Pts',(7.33753740077229,0.98524848898628,11.7012171812671));
#16834=CARTESIAN_POINT('Ctrl Pts',(7.30498972907498,1.05936942930224,11.7054493785671));
#16835=CARTESIAN_POINT('Ctrl Pts',(7.26870453044918,1.13201406351384,11.709681575867));
#16836=CARTESIAN_POINT('Ctrl Pts',(7.22883777515172,1.20278007290367,11.713913773167));
#16837=CARTESIAN_POINT('Ctrl Pts',(7.18902800487398,1.27344493028325,11.7181399210194));
#16838=CARTESIAN_POINT('Ctrl Pts',(7.14564707184775,1.34223609465023,11.7223660688718));
#16839=CARTESIAN_POINT('Ctrl Pts',(7.0988986101566,1.40877205804673,11.7265922167241));
#16840=CARTESIAN_POINT('Ctrl Pts',(7.05213876890876,1.47532421769314,11.7308193933096));
#16841=CARTESIAN_POINT('Ctrl Pts',(7.00200997126493,1.53961966245601,11.7350465698951));
#16842=CARTESIAN_POINT('Ctrl Pts',(6.94876160056616,1.60130211213661,11.7392737464805));
#16843=CARTESIAN_POINT('Ctrl Pts',(6.89562147843312,1.66285916761976,11.7434923296425));
#16844=CARTESIAN_POINT('Ctrl Pts',(6.83937473883501,1.72181347324932,11.7477109128044));
#16845=CARTESIAN_POINT('Ctrl Pts',(6.78031090407868,1.77784217961603,11.7519294959663));
#16846=CARTESIAN_POINT('Ctrl Pts',(6.72126645428652,1.83385249715867,11.756146694574));
#16847=CARTESIAN_POINT('Ctrl Pts',(6.65940708232636,1.88693880275201,11.7603638931816));
#16848=CARTESIAN_POINT('Ctrl Pts',(6.5950591456263,1.93681510776859,11.7645810917893));
#16849=CARTESIAN_POINT('Ctrl Pts',(6.53071264156319,1.98669030234337,11.7687981965056));
#16850=CARTESIAN_POINT('Ctrl Pts',(6.46387805088233,2.03335535468002,11.7730153012219));
#16851=CARTESIAN_POINT('Ctrl Pts',(6.39491364406077,2.07656548154942,11.7772324059383));
#16852=CARTESIAN_POINT('Ctrl Pts',(6.32566742255814,2.11995218135962,11.7814667433413));
#16853=CARTESIAN_POINT('Ctrl Pts',(6.25427433491571,2.1598553990506,11.7857010807444));
#16854=CARTESIAN_POINT('Ctrl Pts',(6.18112357072248,2.19607303051205,11.7899354181475));
#16855=CARTESIAN_POINT('Ctrl Pts',(6.10816496399789,2.2321955230032,11.7941586325013));
#16856=CARTESIAN_POINT('Ctrl Pts',(6.03345834856939,2.26465161919133,11.7983818468551));
#16857=CARTESIAN_POINT('Ctrl Pts',(5.95740983617412,2.29328916701726,11.8026050612089));
#16858=CARTESIAN_POINT('Ctrl Pts',(5.88106088034333,2.32203985266775,11.8068449601366));
#16859=CARTESIAN_POINT('Ctrl Pts',(5.80335985434953,2.34694162065989,11.8110848590643));
#16860=CARTESIAN_POINT('Ctrl Pts',(5.72473115689336,2.36789154966326,11.8153247579921));
#16861=CARTESIAN_POINT('Ctrl Pts',(5.6461024594372,2.38884147866663,11.8195646569198));
#16862=CARTESIAN_POINT('Ctrl Pts',(5.5665465603225,2.40583953184433,11.8238045558475));
#16863=CARTESIAN_POINT('Ctrl Pts',(5.48649434798162,2.41883499352721,11.8280444547753));
#16864=CARTESIAN_POINT('Ctrl Pts',(5.40658498862843,2.43180726483879,11.8322767876132));
#16865=CARTESIAN_POINT('Ctrl Pts',(5.32588318148657,2.44083959441903,11.8365091204511));
#16866=CARTESIAN_POINT('Ctrl Pts',(5.2448114322562,2.44584423015004,11.840741453289));
#16867=CARTESIAN_POINT('Ctrl Pts',(5.16385550657287,2.45084171598399,11.8449677395841));
#16868=CARTESIAN_POINT('Ctrl Pts',(5.08253114837649,2.4518229080577,11.8491940258792));
#16869=CARTESIAN_POINT('Ctrl Pts',(5.00126930042078,2.44875137436854,11.8534203121744));
#16870=CARTESIAN_POINT('Ctrl Pts',(4.91999099271485,2.44567921853408,11.8576474545122));
#16871=CARTESIAN_POINT('Ctrl Pts',(4.83877568474453,2.43855264724011,11.8618745968501));
#16872=CARTESIAN_POINT('Ctrl Pts',(4.75805795456608,2.42738733904082,11.866101739188));
#16873=CARTESIAN_POINT('Ctrl Pts',(4.67750090536055,2.4162442570932,11.8703204667533));
#16874=CARTESIAN_POINT('Ctrl Pts',(4.59743991853169,2.40107854053588,11.8745391943186));
#16875=CARTESIAN_POINT('Ctrl Pts',(4.51830338163993,2.38195773173578,11.8787579218839));
#16876=CARTESIAN_POINT('Ctrl Pts',(4.43919278099187,2.36284318959803,11.8829752668015));
#16877=CARTESIAN_POINT('Ctrl Pts',(4.36100647987066,2.3397762384881,11.8871926117192));
#16878=CARTESIAN_POINT('Ctrl Pts',(4.28416194662076,2.31287537485409,11.8914099566368));
#16879=CARTESIAN_POINT('Ctrl Pts',(4.20731909329354,2.28597509930839,11.8956272093577));
#16880=CARTESIAN_POINT('Ctrl Pts',(4.13181838766841,2.25524123248628,11.8998444620787));
#16881=CARTESIAN_POINT('Ctrl Pts',(4.05806005722665,2.22084145499663,11.9040617147996));
#16882=CARTESIAN_POINT('Ctrl Pts',(3.98400588791538,2.18630370270164,11.9082958825899));
#16883=CARTESIAN_POINT('Ctrl Pts',(3.91170853201712,2.14807076021067,11.9125300503802));
#16884=CARTESIAN_POINT('Ctrl Pts',(3.84154911436463,2.10635940850739,11.9167642181706));
#16885=CARTESIAN_POINT('Ctrl Pts',(3.77156869803521,2.06475447711647,11.9209875831113));
#16886=CARTESIAN_POINT('Ctrl Pts',(3.70371569113058,2.01968915628265,11.925210948052));
#16887=CARTESIAN_POINT('Ctrl Pts',(3.63833857592227,1.97142163041174,11.9294343129927));
#16888=CARTESIAN_POINT('Ctrl Pts',(3.57271062074898,1.92296891092285,11.9336738822079));
#16889=CARTESIAN_POINT('Ctrl Pts',(3.50957795267431,1.87128967049584,11.937913451423));
#16890=CARTESIAN_POINT('Ctrl Pts',(3.44925756636745,1.81668409930143,11.9421530206381));
#16891=CARTESIAN_POINT('Ctrl Pts',(3.38893718006058,1.762078528107,11.9463925898532));
#16892=CARTESIAN_POINT('Ctrl Pts',(3.33142936163524,1.70454700020993,11.9506321590683));
#16893=CARTESIAN_POINT('Ctrl Pts',(3.27701083306423,1.64442351622122,11.9548717282835));
#16894=CARTESIAN_POINT('Ctrl Pts',(3.22269978240752,1.58441877757217,11.9591029242465));
#16895=CARTESIAN_POINT('Ctrl Pts',(3.17126306813964,1.52160831074434,11.9633341202096));
#16896=CARTESIAN_POINT('Ctrl Pts',(3.12300397143216,1.45629881113922,11.9675653161726));
#16897=CARTESIAN_POINT('Ctrl Pts',(3.07481388079836,1.39108269811716,11.9717904619143));
#16898=CARTESIAN_POINT('Ctrl Pts',(3.02979265752206,1.3233750201322,11.9760156076559));
#16899=CARTESIAN_POINT('Ctrl Pts',(2.98820510569361,1.2535174644043,11.9802407533975));
#16900=CARTESIAN_POINT('Ctrl Pts',(2.94659509957854,1.18362219062113,11.9844681804139));
#16901=CARTESIAN_POINT('Ctrl Pts',(2.90842276915838,1.11157507936504,11.9886956074304));
#16902=CARTESIAN_POINT('Ctrl Pts',(2.87391138256914,1.03774958988234,11.9929230344468));
#16903=CARTESIAN_POINT('Ctrl Pts',(2.83948033164713,0.964095951505664,11.9971406208511));
#16904=CARTESIAN_POINT('Ctrl Pts',(2.80869341764964,0.888672616786132,12.0013582072554));
#16905=CARTESIAN_POINT('Ctrl Pts',(2.78172678220013,0.811875676445236,12.0055757936596));
#16906=CARTESIAN_POINT('Ctrl Pts',(2.75476897252166,0.735103870578877,12.0097919997118));
#16907=CARTESIAN_POINT('Ctrl Pts',(2.73162911231634,0.656959790173955,12.014008205764));
#16908=CARTESIAN_POINT('Ctrl Pts',(2.71243464087164,0.577858063450985,12.0182244118162));
#16909=CARTESIAN_POINT('Ctrl Pts',(2.69324057175096,0.498757994732792,12.0224405294949));
#16910=CARTESIAN_POINT('Ctrl Pts',(2.67799183547715,0.41870077167333,12.0266566471737));
#16911=CARTESIAN_POINT('Ctrl Pts',(2.66676521675643,0.338113288307206,12.0308727648524));
#16912=CARTESIAN_POINT('Ctrl Pts',(2.6554869344874,0.257154951040742,12.0351082845974));
#16913=CARTESIAN_POINT('Ctrl Pts',(2.64826795746175,0.175661927664486,12.0393438043423));
#16914=CARTESIAN_POINT('Ctrl Pts',(2.6451335020842,0.0940725355818836,12.0435793240872));
#16915=CARTESIAN_POINT('Ctrl Pts',(2.64200886630936,0.0127387462499724,
12.0478015748217));
#16916=CARTESIAN_POINT('Ctrl Pts',(2.64294314827754,-0.0686903414125342,
12.0520238255562));
#16917=CARTESIAN_POINT('Ctrl Pts',(2.64790900905182,-0.149782078717372,
12.0562460762907));
#16918=CARTESIAN_POINT('Ctrl Pts',(2.65289827868884,-0.231256079124994,
12.0604882305408));
#16919=CARTESIAN_POINT('Ctrl Pts',(2.66195717388358,-0.312389071043011,
12.064730384791));
#16920=CARTESIAN_POINT('Ctrl Pts',(2.67500575227409,-0.392750900092013,
12.0689725390412));
#16921=CARTESIAN_POINT('Ctrl Pts',(2.68805433066461,-0.473112729141016,
12.0732146932913));
#16922=CARTESIAN_POINT('Ctrl Pts',(2.70509243275337,-0.552702949733793,
12.0774568475415));
#16923=CARTESIAN_POINT('Ctrl Pts',(2.72598967865944,-0.631106911300591,
12.0816990017917));
#16924=CARTESIAN_POINT('Ctrl Pts',(2.74684212322271,-0.709342783599845,
12.0859320613407));
#16925=CARTESIAN_POINT('Ctrl Pts',(2.77161505752076,-0.78668975636709,12.0901651208897));
#16926=CARTESIAN_POINT('Ctrl Pts',(2.80021568143163,-0.862726292770211,
12.0943981804387));
#16927=CARTESIAN_POINT('Ctrl Pts',(2.8287754073789,-0.938654099394971,12.09862518685));
#16928=CARTESIAN_POINT('Ctrl Pts',(2.8611517897442,-1.01327476032922,12.1028521932613));
#16929=CARTESIAN_POINT('Ctrl Pts',(2.89720174783176,-1.08618003507352,12.1070791996726));
#16930=CARTESIAN_POINT('Ctrl Pts',(2.9332513227617,-1.15908453494283,12.111306161157));
#16931=CARTESIAN_POINT('Ctrl Pts',(2.97297424750053,-1.2302732431027,12.1155331226415));
#16932=CARTESIAN_POINT('Ctrl Pts',(3.01617852991393,-1.29935616318051,12.119760084126));
#16933=CARTESIAN_POINT('Ctrl Pts',(3.05930579810639,-1.36831593881585,12.1239795107985));
#16934=CARTESIAN_POINT('Ctrl Pts',(3.10590180028734,-1.4351770192821,12.1281989374709));
#16935=CARTESIAN_POINT('Ctrl Pts',(3.15572963307939,-1.49957602133697,12.1324183641434));
#16936=CARTESIAN_POINT('Ctrl Pts',(3.2055410269042,-1.56395377717211,12.1366363987622));
#16937=CARTESIAN_POINT('Ctrl Pts',(3.25858184986589,-1.62587070067144,12.1408544333811));
#16938=CARTESIAN_POINT('Ctrl Pts',(3.31457316612192,-1.68499421110253,12.1450724679999));
#16939=CARTESIAN_POINT('Ctrl Pts',(3.37056312203107,-1.74411628508797,12.1492904001387));
#16940=CARTESIAN_POINT('Ctrl Pts',(3.42950310851249,-1.80044474448912,12.1535083322775));
#16941=CARTESIAN_POINT('Ctrl Pts',(3.49107635611985,-1.85368285454567,12.1577262644163));
#16942=CARTESIAN_POINT('Ctrl Pts',(3.55287444314557,-1.90711536762894,12.1619595986566));
#16943=CARTESIAN_POINT('Ctrl Pts',(3.61732470858141,-1.95743460485067,12.1661929328969));
#16944=CARTESIAN_POINT('Ctrl Pts',(3.68407376652017,-2.00438160847482,12.1704262671372));
#16945=CARTESIAN_POINT('Ctrl Pts',(3.75067584475842,-2.05122523601029,12.174650279685));
#16946=CARTESIAN_POINT('Ctrl Pts',(3.81956618752025,-2.09471124759712,12.1788742922327));
#16947=CARTESIAN_POINT('Ctrl Pts',(3.8903665996224,-2.13462711979391,12.1830983047804));
#16948=CARTESIAN_POINT('Ctrl Pts',(3.96140137881133,-2.17467512351939,12.187336299867));
#16949=CARTESIAN_POINT('Ctrl Pts',(4.0343584686729,-2.21112911292004,12.1915742949536));
#16950=CARTESIAN_POINT('Ctrl Pts',(4.10883484332294,-2.24382271916577,12.1958122900402));
#16951=CARTESIAN_POINT('Ctrl Pts',(4.18331121797297,-2.27651632541149,12.2000502851268));
#16952=CARTESIAN_POINT('Ctrl Pts',(4.25930642045452,-2.30544944046707,12.2042882802134));
#16953=CARTESIAN_POINT('Ctrl Pts',(4.3364030504409,-2.33050616286386,12.2085262753));
#16954=CARTESIAN_POINT('Ctrl Pts',(4.41341479090877,-2.35553529581738,12.2127596040171));
#16955=CARTESIAN_POINT('Ctrl Pts',(4.49181138361709,-2.37678948157706,12.2169929327342));
#16956=CARTESIAN_POINT('Ctrl Pts',(4.57118843361084,-2.39411758617472,12.2212262614513));
#16957=CARTESIAN_POINT('Ctrl Pts',(4.65045234877213,-2.41142099330365,12.2254535564731));
#16958=CARTESIAN_POINT('Ctrl Pts',(4.73069349579421,-2.42480933510125,12.2296808514949));
#16959=CARTESIAN_POINT('Ctrl Pts',(4.81149132896875,-2.43418091584898,12.2339081465167));
#16960=CARTESIAN_POINT('Ctrl Pts',(4.8922814544946,-2.4435516026018,12.2381350382788));
#16961=CARTESIAN_POINT('Ctrl Pts',(4.97362770864029,-2.44890617950953,12.242361930041));
#16962=CARTESIAN_POINT('Ctrl Pts',(5.05509840725034,-2.45019393805116,12.2465888218031));
#16963=CARTESIAN_POINT('Ctrl Pts',(5.1364316409545,-2.45147952376735,12.2508085815621));
#16964=CARTESIAN_POINT('Ctrl Pts',(5.21788843608424,-2.44871196858668,12.2550283413211));
#16965=CARTESIAN_POINT('Ctrl Pts',(5.29903493442271,-2.44189271210886,12.2592481010801));
#16966=CARTESIAN_POINT('Ctrl Pts',(5.38015496866996,-2.43507567957698,12.2634664846601));
#16967=CARTESIAN_POINT('Ctrl Pts',(5.46096444471608,-2.42420960878395,12.2676848682401));
#16968=CARTESIAN_POINT('Ctrl Pts',(5.54103252799396,-2.40934796257631,12.2719032518201));
#16969=CARTESIAN_POINT('Ctrl Pts',(5.62109895630628,-2.39448662355115,12.2761215482084));
#16970=CARTESIAN_POINT('Ctrl Pts',(5.70042356596385,-2.37562995920312,12.2803398445966));
#16971=CARTESIAN_POINT('Ctrl Pts',(5.77858506014438,-2.35288267067502,12.2845581409848));
#16972=CARTESIAN_POINT('Ctrl Pts',(5.85701808554136,-2.33005635859461,12.2887910916367));
#16973=CARTESIAN_POINT('Ctrl Pts',(5.93427944615126,-2.30331246618675,12.2930240422887));
#16974=CARTESIAN_POINT('Ctrl Pts',(6.00995988304162,-2.27280687156679,12.2972569929406));
#16975=CARTESIAN_POINT('Ctrl Pts',(6.08548762263293,-2.24236282682811,12.3014814029425));
#16976=CARTESIAN_POINT('Ctrl Pts',(6.15944040314804,-2.20817247345499,12.3057058129443));
#16977=CARTESIAN_POINT('Ctrl Pts',(6.23143424151941,-2.17043782858016,12.3099302229461));
#16978=CARTESIAN_POINT('Ctrl Pts',(6.30364640890595,-2.13258874935872,12.3141674439231));
#16979=CARTESIAN_POINT('Ctrl Pts',(6.37388733787049,-2.09117409937537,12.3184046649001));
#16980=CARTESIAN_POINT('Ctrl Pts',(6.44179859361809,-2.04644160725183,12.3226418858771));
#16981=CARTESIAN_POINT('Ctrl Pts',(6.50970984936569,-2.00170911512828,12.3268791068541));
#16982=CARTESIAN_POINT('Ctrl Pts',(6.57529109347342,-1.95365910527841,12.3311163278311));
#16983=CARTESIAN_POINT('Ctrl Pts',(6.63821840765248,-1.90257875267492,12.3353535488081));
#16984=CARTESIAN_POINT('Ctrl Pts',(6.70017387946119,-1.85228727929821,12.3395253306204));
#16985=CARTESIAN_POINT('Ctrl Pts',(6.75980227254098,-1.79885891033061,12.3436971124327));
#16986=CARTESIAN_POINT('Ctrl Pts',(6.81676197200124,-1.74254006207211,12.347868894245));
#16987=CARTESIAN_POINT('Ctrl Pts',(6.87403079799516,-1.68591556524967,12.3520633167745));
#16988=CARTESIAN_POINT('Ctrl Pts',(6.92860144877801,-1.62636936367116,12.3562577393041));
#16989=CARTESIAN_POINT('Ctrl Pts',(6.98015816947068,-1.56419485856316,12.3604521618336));
#16990=CARTESIAN_POINT('Ctrl Pts',(7.03130373206592,-1.50251618699318,12.3646131343926));
#16991=CARTESIAN_POINT('Ctrl Pts',(7.07948293519092,-1.43825134120083,12.3687741069517));
#16992=CARTESIAN_POINT('Ctrl Pts',(7.12442385468376,-1.37172420517886,12.3729350795107));
#16993=CARTESIAN_POINT('Ctrl Pts',(7.16933765947029,-1.30523720771605,12.3770935415837));
#16994=CARTESIAN_POINT('Ctrl Pts',(7.21101678911364,-1.2364910238531,12.3812520036568));
#16995=CARTESIAN_POINT('Ctrl Pts',(7.24923085639673,-1.16584095654534,12.3854104657298));
#16996=CARTESIAN_POINT('Ctrl Pts',(7.28743434581261,-1.09521044557071,12.3895677767173));
#16997=CARTESIAN_POINT('Ctrl Pts',(7.32217444962915,-1.02267751879693,12.3937250877048));
#16998=CARTESIAN_POINT('Ctrl Pts',(7.35326605810788,-0.9486232630345,12.3978823986923));
#16999=CARTESIAN_POINT('Ctrl Pts',(7.38483437914912,-0.873433569263015,
12.4021034517141));
#17000=CARTESIAN_POINT('Ctrl Pts',(7.41264114922194,-0.796675953919252,
12.4063245047359));
#17001=CARTESIAN_POINT('Ctrl Pts',(7.43654351869195,-0.71876998505293,12.4105455577577));
#17002=CARTESIAN_POINT('Ctrl Pts',(7.46010721060141,-0.641967881789596,
12.4147068018162));
#17003=CARTESIAN_POINT('Ctrl Pts',(7.47987637177058,-0.564050245634618,
12.4188680458746));
#17004=CARTESIAN_POINT('Ctrl Pts',(7.49576514167452,-0.485431931733643,
12.423029289933));
#17005=CARTESIAN_POINT('Ctrl Pts',(7.51199646209124,-0.405118663226077,
12.4272802474365));
#17006=CARTESIAN_POINT('Ctrl Pts',(7.52417803290927,-0.324074672379063,
12.43153120494));
#17007=CARTESIAN_POINT('Ctrl Pts',(7.53227410577428,-0.242748265636235,
12.4357821624435));
#17008=CARTESIAN_POINT('Ctrl Pts',(7.54037017863928,-0.161421858893407,
12.440033119947));
#17009=CARTESIAN_POINT('Ctrl Pts',(7.54438079120497,-0.0798135650836431,
12.4442840774505));
#17010=CARTESIAN_POINT('Ctrl Pts',(7.54432661325899,0.0016301205695403,
12.448535034954));
#17011=CARTESIAN_POINT('',(4.01701573214483,2.20564849764805,12.7063139509272));
#17012=CARTESIAN_POINT('Ctrl Pts',(7.54716442798305,0.00163200833986455,
12.448535034954));
#17013=CARTESIAN_POINT('Ctrl Pts',(7.54778238923041,0.0888794869590354,
12.4530836307415));
#17014=CARTESIAN_POINT('Ctrl Pts',(7.50402124842324,0.986360506775624,12.4999079843645));
#17015=CARTESIAN_POINT('Ctrl Pts',(6.43805666178856,2.52634553668383,12.5858342896898));
#17016=CARTESIAN_POINT('Ctrl Pts',(4.69254186919481,2.53083748163268,12.6672119992262));
#17017=CARTESIAN_POINT('Ctrl Pts',(4.01701573214483,2.20564849764805,12.7063139509272));
#17018=CARTESIAN_POINT('',(6.16891561580437,2.2020751695661,12.7063625311661));
#17019=CARTESIAN_POINT('Origin',(5.09382715545311,0.,12.7063625311661));
#17020=CARTESIAN_POINT('',(7.54449188652341,0.00262105217720109,12.5641900273781));
#17021=CARTESIAN_POINT('Ctrl Pts',(6.16891561580437,2.2020751695661,12.7063625311661));
#17022=CARTESIAN_POINT('Ctrl Pts',(6.90007729696916,1.84511029528064,12.66408677333));
#17023=CARTESIAN_POINT('Ctrl Pts',(7.49776343645215,1.00822659690667,12.616695938734));
#17024=CARTESIAN_POINT('Ctrl Pts',(7.54732991511167,0.100698102860481,12.569305104138));
#17025=CARTESIAN_POINT('Ctrl Pts',(7.5465663696151,0.00262327089294606,
12.5641900273781));
#17026=CARTESIAN_POINT('',(7.54432697499987,0.000940426119431302,11.7641900274209));
#17027=CARTESIAN_POINT('Ctrl Pts',(7.54432575390545,0.00262087449387521,
12.5641900273781));
#17028=CARTESIAN_POINT('Ctrl Pts',(7.54441039363029,-0.0765166529131762,
12.5600588096074));
#17029=CARTESIAN_POINT('Ctrl Pts',(7.54065735796923,-0.155830075205808,
12.5559275918367));
#17030=CARTESIAN_POINT('Ctrl Pts',(7.53304219039848,-0.234904796239755,
12.551796374066));
#17031=CARTESIAN_POINT('Ctrl Pts',(7.52543169538823,-0.313930998128938,
12.5476676911528));
#17032=CARTESIAN_POINT('Ctrl Pts',(7.51396376930776,-0.392718305017181,
12.5435390082396));
#17033=CARTESIAN_POINT('Ctrl Pts',(7.49866605561368,-0.470850416028822,
12.5394103253264));
#17034=CARTESIAN_POINT('Ctrl Pts',(7.48339408899119,-0.548851025490896,
12.5352885912617));
#17035=CARTESIAN_POINT('Ctrl Pts',(7.46430526170117,-0.626198157536901,
12.531166857197));
#17036=CARTESIAN_POINT('Ctrl Pts',(7.44147889145808,-0.702482438522753,
12.5270451231323));
#17037=CARTESIAN_POINT('Ctrl Pts',(7.41866359048101,-0.77872972672389,12.5229253878336));
#17038=CARTESIAN_POINT('Ctrl Pts',(7.39211447967603,-0.853914719635981,
12.5188056525348));
#17039=CARTESIAN_POINT('Ctrl Pts',(7.36196141833813,-0.927640671557172,
12.514685917236));
#17040=CARTESIAN_POINT('Ctrl Pts',(7.33181284675423,-1.00135564577416,12.5105667953608));
#17041=CARTESIAN_POINT('Ctrl Pts',(7.29806157496909,-1.07361155940243,12.5064476734855));
#17042=CARTESIAN_POINT('Ctrl Pts',(7.26088591303975,-1.14403085236677,12.5023285516103));
#17043=CARTESIAN_POINT('Ctrl Pts',(7.22356652198715,-1.21472240149854,12.4981935043219));
#17044=CARTESIAN_POINT('Ctrl Pts',(7.18279642730905,-1.28356265622267,12.4940584570335));
#17045=CARTESIAN_POINT('Ctrl Pts',(7.13880198786701,-1.35019560982612,12.4899234097451));
#17046=CARTESIAN_POINT('Ctrl Pts',(7.09492050179105,-1.41665748689135,12.4857989789691));
#17047=CARTESIAN_POINT('Ctrl Pts',(7.04783153069711,-1.48092301251295,12.4816745481931));
#17048=CARTESIAN_POINT('Ctrl Pts',(6.99780120556054,-1.54267075765295,12.477550117417));
#17049=CARTESIAN_POINT('Ctrl Pts',(6.94757770919841,-1.60465691594679,12.4734097618725));
#17050=CARTESIAN_POINT('Ctrl Pts',(6.89439044087583,-1.66410545488232,12.4692694063279));
#17051=CARTESIAN_POINT('Ctrl Pts',(6.83854558294449,-1.72072887427741,12.4651290507833));
#17052=CARTESIAN_POINT('Ctrl Pts',(6.78270072501315,-1.7773522936725,12.4609886952388));
#17053=CARTESIAN_POINT('Ctrl Pts',(6.72419868715357,-1.8311503181936,12.4568483396942));
#17054=CARTESIAN_POINT('Ctrl Pts',(6.66337686356165,-1.88187777599301,12.4527079841497));
#17055=CARTESIAN_POINT('Ctrl Pts',(6.60111156302209,-1.93380914238347,12.4484693660501));
#17056=CARTESIAN_POINT('Ctrl Pts',(6.53615211630521,-1.9827420585461,12.4442307479506));
#17057=CARTESIAN_POINT('Ctrl Pts',(6.46881878398513,-2.02838563184293,12.4399921298511));
#17058=CARTESIAN_POINT('Ctrl Pts',(6.40158139194111,-2.07396416963846,12.4357595511703));
#17059=CARTESIAN_POINT('Ctrl Pts',(6.33197721295795,-2.11626241632434,12.4315269724895));
#17060=CARTESIAN_POINT('Ctrl Pts',(6.26035982944157,-2.15502941291235,12.4272943938088));
#17061=CARTESIAN_POINT('Ctrl Pts',(6.18882535891484,-2.19375152811222,12.4230667152756));
#17062=CARTESIAN_POINT('Ctrl Pts',(6.11528272169359,-2.22895029989725,12.4188390367425));
#17063=CARTESIAN_POINT('Ctrl Pts',(6.0401135269968,-2.26041862340379,12.4146113582094));
#17064=CARTESIAN_POINT('Ctrl Pts',(5.96499220158081,-2.29186690723823,12.4103863719484));
#17065=CARTESIAN_POINT('Ctrl Pts',(5.88824680106865,-2.3195892808155,12.4061613856875));
#17066=CARTESIAN_POINT('Ctrl Pts',(5.81028151198016,-2.34342557061525,12.4019363994265));
#17067=CARTESIAN_POINT('Ctrl Pts',(5.73234222836054,-2.36725390977569,12.3977128224177));
#17068=CARTESIAN_POINT('Ctrl Pts',(5.65318430674542,-2.38719860433681,12.3934892454088));
#17069=CARTESIAN_POINT('Ctrl Pts',(5.57322846081274,-2.40314890059261,12.3892656684));
#17070=CARTESIAN_POINT('Ctrl Pts',(5.4932750370186,-2.41909871365889,12.3850422193379));
#17071=CARTESIAN_POINT('Ctrl Pts',(5.41252419124509,-2.43105427952477,12.3808187702757));
#17072=CARTESIAN_POINT('Ctrl Pts',(5.33140684309925,-2.43895595327549,12.3765953212136));
#17073=CARTESIAN_POINT('Ctrl Pts',(5.25021173823486,-2.44686520133968,12.3723678236767));
#17074=CARTESIAN_POINT('Ctrl Pts',(5.16864989101269,-2.45071274847713,12.3681403261398));
#17075=CARTESIAN_POINT('Ctrl Pts',(5.08715683549386,-2.45049092159747,12.3639128286029));
#17076=CARTESIAN_POINT('Ctrl Pts',(5.00562695682094,-2.45026899448393,12.3596834208444));
#17077=CARTESIAN_POINT('Ctrl Pts',(4.92416639489778,-2.4459740532487,12.3554540130859));
#17078=CARTESIAN_POINT('Ctrl Pts',(4.84320769004459,-2.4376505355687,12.3512246053274));
#17079=CARTESIAN_POINT('Ctrl Pts',(4.76210461051928,-2.42931217445539,12.346987655213));
#17080=CARTESIAN_POINT('Ctrl Pts',(4.68150563575141,-2.41693094920283,12.3427507050987));
#17081=CARTESIAN_POINT('Ctrl Pts',(4.60183511267227,-2.40060285758397,12.3385137549844));
#17082=CARTESIAN_POINT('Ctrl Pts',(4.52265227094791,-2.38437471391994,12.3343027402034));
#17083=CARTESIAN_POINT('Ctrl Pts',(4.44438695422857,-2.36424809348003,12.3300917254224));
#17084=CARTESIAN_POINT('Ctrl Pts',(4.36743897176698,-2.34036545364205,12.3258807106414));
#17085=CARTESIAN_POINT('Ctrl Pts',(4.28997218984913,-2.31632179203111,12.3216413043145));
#17086=CARTESIAN_POINT('Ctrl Pts',(4.21356169799378,-2.28838468318746,12.3174018979875));
#17087=CARTESIAN_POINT('Ctrl Pts',(4.13862575067865,-2.2566657985437,12.3131624916606));
#17088=CARTESIAN_POINT('Ctrl Pts',(4.06379404581372,-2.22499103763991,12.3089289827183));
#17089=CARTESIAN_POINT('Ctrl Pts',(3.99043323388083,-2.18954512970591,12.304695473776));
#17090=CARTESIAN_POINT('Ctrl Pts',(3.91894603217246,-2.15048938526997,12.3004619648337));
#17091=CARTESIAN_POINT('Ctrl Pts',(3.84753799270652,-2.11147688969865,12.2962331439202));
#17092=CARTESIAN_POINT('Ctrl Pts',(3.77799984390751,-2.06886272354524,12.2920043230067));
#17093=CARTESIAN_POINT('Ctrl Pts',(3.71071262565826,-2.02285551818967,12.2877755020932));
#17094=CARTESIAN_POINT('Ctrl Pts',(3.64346620254492,-1.97687620624748,12.2835492450444));
#17095=CARTESIAN_POINT('Ctrl Pts',(3.57846838168398,-1.92750819977463,12.2793229879955));
#17096=CARTESIAN_POINT('Ctrl Pts',(3.51607296767334,-1.87500452611278,12.2750967309467));
#17097=CARTESIAN_POINT('Ctrl Pts',(3.45369648481703,-1.82251678239007,12.2708717561705));
#17098=CARTESIAN_POINT('Ctrl Pts',(3.39392119442706,-1.7668955588495,12.2666467813942));
#17099=CARTESIAN_POINT('Ctrl Pts',(3.33706830103246,-1.70843453998526,12.2624218066179));
#17100=CARTESIAN_POINT('Ctrl Pts',(3.28021543825759,-1.64997355260686,12.2581968341171));
#17101=CARTESIAN_POINT('Ctrl Pts',(3.22628529105744,-1.58867310563953,12.2539718616163));
#17102=CARTESIAN_POINT('Ctrl Pts',(3.17556162418357,-1.52486314190592,12.2497468891155));
#17103=CARTESIAN_POINT('Ctrl Pts',(3.1247870695095,-1.46098916173017,12.2455176779708));
#17104=CARTESIAN_POINT('Ctrl Pts',(3.07722571031335,-1.39460099831619,12.2412884668262));
#17105=CARTESIAN_POINT('Ctrl Pts',(3.03312013232558,-1.32606063769078,12.2370592556816));
#17106=CARTESIAN_POINT('Ctrl Pts',(2.9889935273383,-1.25748760096871,12.2328280282927));
#17107=CARTESIAN_POINT('Ctrl Pts',(2.94832621731021,-1.1867607243928,12.2285968009038));
#17108=CARTESIAN_POINT('Ctrl Pts',(2.91131535792414,-1.11426769837721,12.2243655735148));
#17109=CARTESIAN_POINT('Ctrl Pts',(2.87423710327715,-1.04164266552676,12.2201266412339));
#17110=CARTESIAN_POINT('Ctrl Pts',(2.84082879585868,-0.967245479317497,
12.215887708953));
#17111=CARTESIAN_POINT('Ctrl Pts',(2.81123981787899,-0.891484882847885,
12.2116487766721));
#17112=CARTESIAN_POINT('Ctrl Pts',(2.78193344231364,-0.816447870933587,
12.2074503301591));
#17113=CARTESIAN_POINT('Ctrl Pts',(2.75637379469379,-0.740073828005492,
12.2032518836462));
#17114=CARTESIAN_POINT('Ctrl Pts',(2.73465698606719,-0.662771726825782,
12.1990534371333));
#17115=CARTESIAN_POINT('Ctrl Pts',(2.71279593603056,-0.58495619090229,12.1948271048542));
#17116=CARTESIAN_POINT('Ctrl Pts',(2.69474720806299,-0.505908885358544,
12.1906007725752));
#17117=CARTESIAN_POINT('Ctrl Pts',(2.68064634693347,-0.426038302729327,
12.1863744402962));
#17118=CARTESIAN_POINT('Ctrl Pts',(2.66656593634664,-0.346283556767435,
12.182154237486));
#17119=CARTESIAN_POINT('Ctrl Pts',(2.65642210231356,-0.265708359974596,
12.1779340346759));
#17120=CARTESIAN_POINT('Ctrl Pts',(2.65030039347467,-0.184735523100296,
12.1737138318657));
#17121=CARTESIAN_POINT('Ctrl Pts',(2.64416642725262,-0.103600555828764,
12.1694851790223));
#17122=CARTESIAN_POINT('Ctrl Pts',(2.64207082699148,-0.0220668115723537,
12.165256526179));
#17123=CARTESIAN_POINT('Ctrl Pts',(2.64404793756445,0.0594309145210368,
12.1610278733356));
#17124=CARTESIAN_POINT('Ctrl Pts',(2.64601748951117,0.140617069344841,12.1568153869155));
#17125=CARTESIAN_POINT('Ctrl Pts',(2.65202867048672,0.221767012350393,12.1526029004954));
#17126=CARTESIAN_POINT('Ctrl Pts',(2.66206336155539,0.302448509151835,12.1483904140753));
#17127=CARTESIAN_POINT('Ctrl Pts',(2.67209465002971,0.383102648219714,12.1441793560382));
#17128=CARTESIAN_POINT('Ctrl Pts',(2.68614668199914,0.463288194291076,12.1399682980012));
#17129=CARTESIAN_POINT('Ctrl Pts',(2.70414947098843,0.54257793391506,12.1357572399641));
#17130=CARTESIAN_POINT('Ctrl Pts',(2.72215170586108,0.621865233041374,12.1315463115413));
#17131=CARTESIAN_POINT('Ctrl Pts',(2.74410435173223,0.700256326194733,12.1273353831184));
#17132=CARTESIAN_POINT('Ctrl Pts',(2.769886593912,0.777335523711612,12.1231244546956));
#17133=CARTESIAN_POINT('Ctrl Pts',(2.79585616513128,0.85497476453021,12.1188829304397));
#17134=CARTESIAN_POINT('Ctrl Pts',(2.82571107356269,0.93128250825446,12.1146414061838));
#17135=CARTESIAN_POINT('Ctrl Pts',(2.85927779811455,1.00585258344243,12.1103998819279));
#17136=CARTESIAN_POINT('Ctrl Pts',(2.89265053975843,1.07999171637356,12.1061828695427));
#17137=CARTESIAN_POINT('Ctrl Pts',(2.92969204340042,1.15241281953426,12.1019658571574));
#17138=CARTESIAN_POINT('Ctrl Pts',(2.97018556120639,1.22274144003761,12.0977488447721));
#17139=CARTESIAN_POINT('Ctrl Pts',(3.01103213887281,1.2936832503621,12.093495064581));
#17140=CARTESIAN_POINT('Ctrl Pts',(3.05539095687902,1.36249550563928,12.0892412843898));
#17141=CARTESIAN_POINT('Ctrl Pts',(3.10299605367378,1.42882531269155,12.0849875041986));
#17142=CARTESIAN_POINT('Ctrl Pts',(3.15060115046855,1.49515511974382,12.0807337240074));
#17143=CARTESIAN_POINT('Ctrl Pts',(3.2014521767119,1.55900214351023,12.0764799438162));
#17144=CARTESIAN_POINT('Ctrl Pts',(3.25524434129407,1.62005045769539,12.072226163625));
#17145=CARTESIAN_POINT('Ctrl Pts',(3.30877838497379,1.68080583245204,12.0679927951348));
#17146=CARTESIAN_POINT('Ctrl Pts',(3.36542656841756,1.7390176940597,12.0637594266447));
#17147=CARTESIAN_POINT('Ctrl Pts',(3.42491785484029,1.79435002057236,12.0595260581545));
#17148=CARTESIAN_POINT('Ctrl Pts',(3.48432422738297,1.84960336942596,12.0552987320912));
#17149=CARTESIAN_POINT('Ctrl Pts',(3.54656530581361,1.9019850327265,12.0510714060278));
#17150=CARTESIAN_POINT('Ctrl Pts',(3.61133097407495,1.95119330723513,12.0468440799645));
#17151=CARTESIAN_POINT('Ctrl Pts',(3.67608985291409,2.00039642321209,12.0426171970542));
#17152=CARTESIAN_POINT('Ctrl Pts',(3.74337246252358,2.04642648679026,12.0383903141439));
#17153=CARTESIAN_POINT('Ctrl Pts',(3.81283313979633,2.08902000513435,12.0341634312335));
#17154=CARTESIAN_POINT('Ctrl Pts',(3.88217692046509,2.13154184209205,12.0299436618193));
#17155=CARTESIAN_POINT('Ctrl Pts',(3.95369106289455,2.17063842488001,12.0257238924051));
#17156=CARTESIAN_POINT('Ctrl Pts',(4.02700146581783,2.20609002489341,12.0215041229909));
#17157=CARTESIAN_POINT('Ctrl Pts',(4.1002878200654,2.24152999539724,12.0172857378259));
#17158=CARTESIAN_POINT('Ctrl Pts',(4.17536884687027,2.27332715571786,12.0130673526609));
#17159=CARTESIAN_POINT('Ctrl Pts',(4.25184654972842,2.30130808662888,12.0088489674958));
#17160=CARTESIAN_POINT('Ctrl Pts',(4.32832252564945,2.32928838570465,12.0046306775859));
#17161=CARTESIAN_POINT('Ctrl Pts',(4.40619467843011,2.35345246823344,12.0004123876759));
#17162=CARTESIAN_POINT('Ctrl Pts',(4.48504712189463,2.37367586682355,11.9961940977659));
#17163=CARTESIAN_POINT('Ctrl Pts',(4.56417330661427,2.39396947222362,11.9919611637951));
#17164=CARTESIAN_POINT('Ctrl Pts',(4.64428614693988,2.41029485983171,11.9877282298244));
#17165=CARTESIAN_POINT('Ctrl Pts',(4.72495405036333,2.42257773504617,11.9834952958536));
#17166=CARTESIAN_POINT('Ctrl Pts',(4.80545901304841,2.43483580013576,11.9792709119673));
#17167=CARTESIAN_POINT('Ctrl Pts',(4.88651633050828,2.44306765643798,11.975046528081));
#17168=CARTESIAN_POINT('Ctrl Pts',(4.96769266192047,2.44725158893426,11.9708221441947));
#17169=CARTESIAN_POINT('Ctrl Pts',(5.04911544269933,2.45144822374778,11.9665849351817));
#17170=CARTESIAN_POINT('Ctrl Pts',(5.13065749219384,2.45157233176375,11.9623477261687));
#17171=CARTESIAN_POINT('Ctrl Pts',(5.21188416609952,2.44765454920363,11.9581105171557));
#17172=CARTESIAN_POINT('Ctrl Pts',(5.29311084000522,2.44373676664352,11.9538733081427));
#17173=CARTESIAN_POINT('Ctrl Pts',(5.37402168182735,2.43577720026681,11.9496360991297));
#17174=CARTESIAN_POINT('Ctrl Pts',(5.45419165729818,2.42385801477932,11.9453988901167));
#17175=CARTESIAN_POINT('Ctrl Pts',(5.53428104988045,2.41195080986674,11.9411659401364));
#17176=CARTESIAN_POINT('Ctrl Pts',(5.61392831550511,2.39604775568114,11.936932990156));
#17177=CARTESIAN_POINT('Ctrl Pts',(5.69270414619543,2.37619372105042,11.9327000401757));
#17178=CARTESIAN_POINT('Ctrl Pts',(5.77136776588927,2.35636796718792,11.9284731197545));
#17179=CARTESIAN_POINT('Ctrl Pts',(5.84916196939663,2.33260252326163,11.9242461993334));
#17180=CARTESIAN_POINT('Ctrl Pts',(5.92566501726814,2.30499371401551,11.9200192789123));
#17181=CARTESIAN_POINT('Ctrl Pts',(6.00216925077248,2.27738447689217,11.9157922929829));
#17182=CARTESIAN_POINT('Ctrl Pts',(6.07738183278321,2.24593185252719,11.9115653070536));
#17183=CARTESIAN_POINT('Ctrl Pts',(6.15089363736988,2.21078282579002,11.9073383211243));
#17184=CARTESIAN_POINT('Ctrl Pts',(6.22427348762946,2.17569689186082,11.9031189226714));
#17185=CARTESIAN_POINT('Ctrl Pts',(6.29595823061345,2.13692799014802,11.8988995242185));
#17186=CARTESIAN_POINT('Ctrl Pts',(6.3655601667511,2.09467071349531,11.8946801257656));
#17187=CARTESIAN_POINT('Ctrl Pts',(6.43513949964716,2.05242715990098,11.8904620975631));
#17188=CARTESIAN_POINT('Ctrl Pts',(6.50263697224862,2.00669772199978,11.8862440693606));
#17189=CARTESIAN_POINT('Ctrl Pts',(6.56769077542748,1.95772221719938,11.8820260411582));
#17190=CARTESIAN_POINT('Ctrl Pts',(6.63274333409962,1.90874764932106,11.8778080936483));
#17191=CARTESIAN_POINT('Ctrl Pts',(6.69535194593625,1.85652741830497,11.8735901461385));
#17192=CARTESIAN_POINT('Ctrl Pts',(6.7551861750095,1.80134295961058,11.8693721986287));
#17193=CARTESIAN_POINT('Ctrl Pts',(6.81523934965934,1.74595656979225,11.8651388167937));
#17194=CARTESIAN_POINT('Ctrl Pts',(6.87249744720056,1.68758453051007,11.8609054349587));
#17195=CARTESIAN_POINT('Ctrl Pts',(6.92666345787223,1.62654890443989,11.8566720531237));
#17196=CARTESIAN_POINT('Ctrl Pts',(6.98071046469252,1.56564737490892,11.8524479721165));
#17197=CARTESIAN_POINT('Ctrl Pts',(7.03167869416211,1.50209433807564,11.8482238911094));
#17198=CARTESIAN_POINT('Ctrl Pts',(7.07931449339184,1.43624172091085,11.8439998101023));
#17199=CARTESIAN_POINT('Ctrl Pts',(7.12710762354254,1.37017160654704,11.8397617778533));
#17200=CARTESIAN_POINT('Ctrl Pts',(7.17154602850335,1.30178709692435,11.8355237456044));
#17201=CARTESIAN_POINT('Ctrl Pts',(7.21241913883921,1.23146995819311,11.8312857133554));
#17202=CARTESIAN_POINT('Ctrl Pts',(7.25329224917508,1.16115281946187,11.8270476811065));
#17203=CARTESIAN_POINT('Ctrl Pts',(7.29059990638921,1.0889034935897,11.8228096488575));
#17204=CARTESIAN_POINT('Ctrl Pts',(7.3241800758682,1.01512368724007,11.8185716166086));
#17205=CARTESIAN_POINT('Ctrl Pts',(7.36071057463849,0.934861640712458,11.8139612339255));
#17206=CARTESIAN_POINT('Ctrl Pts',(7.39294885099948,0.852528858115445,11.8093508512425));
#17207=CARTESIAN_POINT('Ctrl Pts',(7.42067707427349,0.768582920240606,11.8047404685595));
#17208=CARTESIAN_POINT('Ctrl Pts',(7.4483340584941,0.68485265536771,11.8001419308221));
#17209=CARTESIAN_POINT('Ctrl Pts',(7.47150396342862,0.599517796048167,11.7955433930847));
#17210=CARTESIAN_POINT('Ctrl Pts',(7.49001656496528,0.513056101943753,11.7909448553474));
#17211=CARTESIAN_POINT('Ctrl Pts',(7.50844941034667,0.426966902882021,11.7863661290714));
#17212=CARTESIAN_POINT('Ctrl Pts',(7.52226486289349,0.339760859350498,11.7817874027954));
#17213=CARTESIAN_POINT('Ctrl Pts',(7.53134272764655,0.25192873062537,11.7772086765193));
#17214=CARTESIAN_POINT('Ctrl Pts',(7.53994639663354,0.168684643768949,11.7728691268199));
#17215=CARTESIAN_POINT('Ctrl Pts',(7.54429476214579,0.0848785383195788,
11.7685295771204));
#17216=CARTESIAN_POINT('Ctrl Pts',(7.54432697499987,0.000940426119398955,
11.7641900274209));
#17217=CARTESIAN_POINT('',(7.54432616501525,-0.00220321015044804,10.9641900273343));
#17218=CARTESIAN_POINT('Ctrl Pts',(7.54432697500019,0.000940425291412725,
11.7641900273781));
#17219=CARTESIAN_POINT('Ctrl Pts',(7.54435894248202,-0.0823583855581014,
11.7598835291724));
#17220=CARTESIAN_POINT('Ctrl Pts',(7.54013925275364,-0.165631393861959,
11.7555770309666));
#17221=CARTESIAN_POINT('Ctrl Pts',(7.5317020525233,-0.248427527128179,11.7512705327609));
#17222=CARTESIAN_POINT('Ctrl Pts',(7.52325973069101,-0.331273919820025,
11.7469614203977));
#17223=CARTESIAN_POINT('Ctrl Pts',(7.51059484986504,-0.413642427628778,
11.7426523080346));
#17224=CARTESIAN_POINT('Ctrl Pts',(7.49379315404187,-0.495089341046485,
11.7383431956714));
#17225=CARTESIAN_POINT('Ctrl Pts',(7.47696331328709,-0.576672688180899,
11.7340268650087));
#17226=CARTESIAN_POINT('Ctrl Pts',(7.45598290886903,-0.657330930030507,
11.729710534346));
#17227=CARTESIAN_POINT('Ctrl Pts',(7.43098835149548,-0.736632740050166,
11.7253942036833));
#17228=CARTESIAN_POINT('Ctrl Pts',(7.40597111894622,-0.816006493031197,
11.7210739572259));
#17229=CARTESIAN_POINT('Ctrl Pts',(7.37693263106896,-0.89402095405243,11.7167537107685));
#17230=CARTESIAN_POINT('Ctrl Pts',(7.34405763962233,-0.970264406291163,
11.7124334643111));
#17231=CARTESIAN_POINT('Ctrl Pts',(7.31111457303057,-1.04666573793454,11.708104271801));
#17232=CARTESIAN_POINT('Ctrl Pts',(7.27431932589656,-1.12128834332108,11.703775079291));
#17233=CARTESIAN_POINT('Ctrl Pts',(7.23390285759931,-1.1937446289234,11.6994458867809));
#17234=CARTESIAN_POINT('Ctrl Pts',(7.20993617133476,-1.23671070532952,11.696878705554));
#17235=CARTESIAN_POINT('Ctrl Pts',(7.18469695746452,-1.27891555142926,11.6943115243272));
#17236=CARTESIAN_POINT('Ctrl Pts',(7.15824029078737,-1.32028355161283,11.6917443431004));
#17237=CARTESIAN_POINT('Ctrl Pts',(7.1146230199284,-1.388484103516,11.6875120095157));
#17238=CARTESIAN_POINT('Ctrl Pts',(7.06754118944877,-1.45464801043107,11.6832796759311));
#17239=CARTESIAN_POINT('Ctrl Pts',(7.01721113515328,-1.5184018956234,11.6790473423465));
#17240=CARTESIAN_POINT('Ctrl Pts',(6.96695298744288,-1.58206469559369,11.6748210554999));
#17241=CARTESIAN_POINT('Ctrl Pts',(6.91345611845769,-1.64332395079541,11.6705947686533));
#17242=CARTESIAN_POINT('Ctrl Pts',(6.85698073508804,-1.70183421772525,11.6663684818068));
#17243=CARTESIAN_POINT('Ctrl Pts',(6.8004939220552,-1.76035632614434,11.6621413396311));
#17244=CARTESIAN_POINT('Ctrl Pts',(6.7410276628384,-1.81612795572645,11.6579141974555));
#17245=CARTESIAN_POINT('Ctrl Pts',(6.67888342250527,-1.86883570178833,11.6536870552799));
#17246=CARTESIAN_POINT('Ctrl Pts',(6.61686288630514,-1.92143852797358,11.6494683276405));
#17247=CARTESIAN_POINT('Ctrl Pts',(6.55217535804114,-1.97098933681526,11.6452496000011));
#17248=CARTESIAN_POINT('Ctrl Pts',(6.48515682533867,-2.0172139201622,11.6410308723616));
#17249=CARTESIAN_POINT('Ctrl Pts',(6.41816026017511,-2.06342335187432,11.6368135275496));
#17250=CARTESIAN_POINT('Ctrl Pts',(6.34883459011881,-2.10630845969896,11.6325961827375));
#17251=CARTESIAN_POINT('Ctrl Pts',(6.27754649415294,-2.14563714947053,11.6283788379255));
#17252=CARTESIAN_POINT('Ctrl Pts',(6.20625995967156,-2.18496497779198,11.6241615854896));
#17253=CARTESIAN_POINT('Ctrl Pts',(6.13301149212449,-2.22073631951311,11.6199443330537));
#17254=CARTESIAN_POINT('Ctrl Pts',(6.05819292752296,-2.25276472532311,11.6157270806178));
#17255=CARTESIAN_POINT('Ctrl Pts',(5.98307427009332,-2.28492159517049,11.6114929130323));
#17256=CARTESIAN_POINT('Ctrl Pts',(5.90637332325196,-2.31330524527914,11.6072587454468));
#17257=CARTESIAN_POINT('Ctrl Pts',(5.82850577622104,-2.33777620275905,11.6030245778614));
#17258=CARTESIAN_POINT('Ctrl Pts',(5.75083690615525,-2.36218472324497,11.5988012136413));
#17259=CARTESIAN_POINT('Ctrl Pts',(5.67200784425064,-2.38270041420456,11.5945778494213));
#17260=CARTESIAN_POINT('Ctrl Pts',(5.59244336822967,-2.39923573713722,11.5903544852012));
#17261=CARTESIAN_POINT('Ctrl Pts',(5.51257360332114,-2.41583450610252,11.5861149159331));
#17262=CARTESIAN_POINT('Ctrl Pts',(5.43196323625491,-2.42842223747161,11.5818753466649));
#17263=CARTESIAN_POINT('Ctrl Pts',(5.35104735266986,-2.43696286802729,11.5776357773967));
#17264=CARTESIAN_POINT('Ctrl Pts',(5.2701314690848,-2.44550349858296,11.5733962081285));
#17265=CARTESIAN_POINT('Ctrl Pts',(5.18891053852849,-2.44999706453427,11.5691566388603));
#17266=CARTESIAN_POINT('Ctrl Pts',(5.10781798894077,-2.45046006018836,11.5649170695921));
#17267=CARTESIAN_POINT('Ctrl Pts',(5.02686672690311,-2.45092224916511,11.5606848869255));
#17268=CARTESIAN_POINT('Ctrl Pts',(4.94574161846151,-2.44736963806486,11.5564527042589));
#17269=CARTESIAN_POINT('Ctrl Pts',(4.86487362920176,-2.43978083704604,11.5522205215923));
#17270=CARTESIAN_POINT('Ctrl Pts',(4.78412117184545,-2.43220287775377,11.5479943852257));
#17271=CARTESIAN_POINT('Ctrl Pts',(4.70362556287672,-2.42060022410224,11.543768248859));
#17272=CARTESIAN_POINT('Ctrl Pts',(4.62381817115424,-2.40500349369358,11.5395421124924));
#17273=CARTESIAN_POINT('Ctrl Pts',(4.54399107403052,-2.38940291226531,11.535314932642));
#17274=CARTESIAN_POINT('Ctrl Pts',(4.46485300016943,-2.3698063056605,11.5310877527917));
#17275=CARTESIAN_POINT('Ctrl Pts',(4.38683091139602,-2.34629634975831,11.5268605729413));
#17276=CARTESIAN_POINT('Ctrl Pts',(4.30896756342745,-2.32283422632741,11.522641993552));
#17277=CARTESIAN_POINT('Ctrl Pts',(4.232216116107,-2.29547477175723,11.5184234141626));
#17278=CARTESIAN_POINT('Ctrl Pts',(4.15698934085871,-2.26435093551021,11.5142048347733));
#17279=CARTESIAN_POINT('Ctrl Pts',(4.08178720342966,-2.23323729275414,11.5099876370276));
#17280=CARTESIAN_POINT('Ctrl Pts',(4.00810917544068,-2.19836189423427,11.5057704392819));
#17281=CARTESIAN_POINT('Ctrl Pts',(3.93634936282974,-2.15990634278057,11.5015532415362));
#17282=CARTESIAN_POINT('Ctrl Pts',(3.86459109838284,-2.12145162097649,11.4973361347733));
#17283=CARTESIAN_POINT('Ctrl Pts',(3.79475137604953,-2.0794171203074,11.4931190280105));
#17284=CARTESIAN_POINT('Ctrl Pts',(3.72719966382234,-2.03403037074646,11.4889019212477));
#17285=CARTESIAN_POINT('Ctrl Pts',(3.65937184074846,-1.98845810740006,11.484667577484));
#17286=CARTESIAN_POINT('Ctrl Pts',(3.59385116959799,-1.93950638628338,11.4804332337204));
#17287=CARTESIAN_POINT('Ctrl Pts',(3.53098073004293,-1.88744835706375,11.4761988899567));
#17288=CARTESIAN_POINT('Ctrl Pts',(3.46827540144395,-1.83552704314364,11.4719756664676));
#17289=CARTESIAN_POINT('Ctrl Pts',(3.4082067189857,-1.78051606215411,11.4677524429785));
#17290=CARTESIAN_POINT('Ctrl Pts',(3.35107903103002,-1.72272436124291,11.4635292194894));
#17291=CARTESIAN_POINT('Ctrl Pts',(3.29372570657613,-1.66470440119003,11.4592893155884));
#17292=CARTESIAN_POINT('Ctrl Pts',(3.23933696398529,-1.60388206723264,11.4550494116875));
#17293=CARTESIAN_POINT('Ctrl Pts',(3.18817963370037,-1.54060305492286,11.4508095077866));
#17294=CARTESIAN_POINT('Ctrl Pts',(3.13702230341543,-1.47732404261306,11.4465696038857));
#17295=CARTESIAN_POINT('Ctrl Pts',(3.0890966103807,-1.41158876603943,11.4423296999848));
#17296=CARTESIAN_POINT('Ctrl Pts',(3.04462434700435,-1.3437701067689,11.4380897960839));
#17297=CARTESIAN_POINT('Ctrl Pts',(3.00023530859849,-1.27607836269198,11.4338578266988));
#17298=CARTESIAN_POINT('Ctrl Pts',(2.9591211361363,-1.20605844318704,11.4296258573137));
#17299=CARTESIAN_POINT('Ctrl Pts',(2.92153406383363,-1.13406039261685,11.4253938879286));
#17300=CARTESIAN_POINT('Ctrl Pts',(2.88400073066575,-1.06216527937874,11.4211679690912));
#17301=CARTESIAN_POINT('Ctrl Pts',(2.84998469543737,-0.988298060653317,
11.4169420502538));
#17302=CARTESIAN_POINT('Ctrl Pts',(2.81969476265982,-0.912837395185082,
11.4127161314163));
#17303=CARTESIAN_POINT('Ctrl Pts',(2.78939540538737,-0.83735325067308,11.4084888977147));
#17304=CARTESIAN_POINT('Ctrl Pts',(2.76282470333167,-0.760275071916644,
11.404261664013));
#17305=CARTESIAN_POINT('Ctrl Pts',(2.74014540308181,-0.682006201257992,
11.4000344303113));
#17306=CARTESIAN_POINT('Ctrl Pts',(2.7175137475928,-0.603901758142695,11.3958160771983));
#17307=CARTESIAN_POINT('Ctrl Pts',(2.69875731349992,-0.524612060407832,
11.3915977240854));
#17308=CARTESIAN_POINT('Ctrl Pts',(2.68398890437622,-0.444555793626262,
11.3873793709724));
#17309=CARTESIAN_POINT('Ctrl Pts',(2.66922534216965,-0.364525800906284,
11.3831624023016));
#17310=CARTESIAN_POINT('Ctrl Pts',(2.65844728992316,-0.283730195416169,
11.3789454336308));
#17311=CARTESIAN_POINT('Ctrl Pts',(2.65171656842196,-0.202598446959399,
11.37472846496));
#17312=CARTESIAN_POINT('Ctrl Pts',(2.64498599611946,-0.121468496935655,
11.370511589766));
#17313=CARTESIAN_POINT('Ctrl Pts',(2.64230261346029,-0.040002881983545,
11.366294714572));
#17314=CARTESIAN_POINT('Ctrl Pts',(2.64367629956648,0.0413646394644267,
11.362077839378));
#17315=CARTESIAN_POINT('Ctrl Pts',(2.645055762863,0.123074361110238,11.3578432296445));
#17316=CARTESIAN_POINT('Ctrl Pts',(2.65052649910699,0.20468469025959,11.353608619911));
#17317=CARTESIAN_POINT('Ctrl Pts',(2.66004573388368,0.285759062889458,11.3493740101774));
#17318=CARTESIAN_POINT('Ctrl Pts',(2.66953884376968,0.366610932432473,11.3451510220415));
#17319=CARTESIAN_POINT('Ctrl Pts',(2.68305814087799,0.44692932916564,11.3409280339056));
#17320=CARTESIAN_POINT('Ctrl Pts',(2.70050976198522,0.526290893065881,11.3367050457697));
#17321=CARTESIAN_POINT('Ctrl Pts',(2.71803342297704,0.605980059649459,11.3324646252374));
#17322=CARTESIAN_POINT('Ctrl Pts',(2.7395218114061,0.684704023793716,11.328224204705));
#17323=CARTESIAN_POINT('Ctrl Pts',(2.76482974318002,0.762050722475371,11.3239837841727));
#17324=CARTESIAN_POINT('Ctrl Pts',(2.79013767495394,0.839397421157049,11.3197433636403));
#17325=CARTESIAN_POINT('Ctrl Pts',(2.81926492454934,0.915366440063504,11.315502943108));
#17326=CARTESIAN_POINT('Ctrl Pts',(2.8520189741217,0.989568758659821,11.3112625225756));
#17327=CARTESIAN_POINT('Ctrl Pts',(2.8847090062452,1.06362604959703,11.3070303899011));
#17328=CARTESIAN_POINT('Ctrl Pts',(2.92113363162592,1.13619986823533,11.3027982572265));
#17329=CARTESIAN_POINT('Ctrl Pts',(2.96113610676575,1.20688820561344,11.2985661245519));
#17330=CARTESIAN_POINT('Ctrl Pts',(3.00108141338179,1.27747552054522,11.2943400401225));
#17331=CARTESIAN_POINT('Ctrl Pts',(3.04459418744791,1.34618230492972,11.2901139556932));
#17332=CARTESIAN_POINT('Ctrl Pts',(3.09147006192824,1.4126274526607,11.2858878712638));
#17333=CARTESIAN_POINT('Ctrl Pts',(3.13835822818122,1.47909002361115,11.2816606786723));
#17334=CARTESIAN_POINT('Ctrl Pts',(3.18861104620899,1.54328935610522,11.2774334860807));
#17335=CARTESIAN_POINT('Ctrl Pts',(3.24197843436488,1.60486964087551,11.2732062934892));
#17336=CARTESIAN_POINT('Ctrl Pts',(3.29523637183308,1.66632363120365,11.2689877704083));
#17337=CARTESIAN_POINT('Ctrl Pts',(3.35159583145433,1.72516893830252,11.2647692473274));
#17338=CARTESIAN_POINT('Ctrl Pts',(3.41076667089988,1.78108328141484,11.2605507242464));
#17339=CARTESIAN_POINT('Ctrl Pts',(3.46991810937903,1.83697929130251,11.2563335843371));
#17340=CARTESIAN_POINT('Ctrl Pts',(3.53187875959856,1.88994592677056,11.2521164444277));
#17341=CARTESIAN_POINT('Ctrl Pts',(3.59632171586831,1.9396978394621,11.2478993045184));
#17342=CARTESIAN_POINT('Ctrl Pts',(3.66076325958014,1.98944866161617,11.2436822570467));
#17343=CARTESIAN_POINT('Ctrl Pts',(3.72768663263984,2.03598461804152,11.239465209575));
#17344=CARTESIAN_POINT('Ctrl Pts',(3.79673309666712,2.07906162791344,11.2352481621033));
#17345=CARTESIAN_POINT('Ctrl Pts',(3.86606383093863,2.12231598954826,11.2310137526836));
#17346=CARTESIAN_POINT('Ctrl Pts',(3.93753478158874,2.1620826022527,11.226779343264));
#17347=CARTESIAN_POINT('Ctrl Pts',(4.01075633896331,2.19816010710506,11.2225449338443));
#17348=CARTESIAN_POINT('Ctrl Pts',(4.08378339192877,2.23414177633174,11.2183217726326));
#17349=CARTESIAN_POINT('Ctrl Pts',(4.15855131738468,2.26645376439695,11.2140986114209));
#17350=CARTESIAN_POINT('Ctrl Pts',(4.23465371604348,2.29494471633045,11.2098754502092));
#17351=CARTESIAN_POINT('Ctrl Pts',(4.31106015789206,2.3235494948983,11.2056354166855));
#17352=CARTESIAN_POINT('Ctrl Pts',(4.38881130635894,2.34830250738448,11.2013953831619));
#17353=CARTESIAN_POINT('Ctrl Pts',(4.46748251584643,2.36910165303981,11.1971553496383));
#17354=CARTESIAN_POINT('Ctrl Pts',(4.5461537253339,2.38990079869514,11.1929153161147));
#17355=CARTESIAN_POINT('Ctrl Pts',(4.62574452584903,2.40674604161226,11.1886752825911));
#17356=CARTESIAN_POINT('Ctrl Pts',(4.70582388448333,2.41958750858834,11.1844352490674));
#17357=CARTESIAN_POINT('Ctrl Pts',(4.78575337372431,2.43240494261888,11.1802031508128));
#17358=CARTESIAN_POINT('Ctrl Pts',(4.86646775897929,2.4412814027134,11.1759710525582));
#17359=CARTESIAN_POINT('Ctrl Pts',(4.94754441548954,2.44612992500169,11.1717389543036));
#17360=CARTESIAN_POINT('Ctrl Pts',(5.02850519965063,2.45097151792593,11.1675129044381));
#17361=CARTESIAN_POINT('Ctrl Pts',(5.10982676678235,2.45179657878873,11.1632868545726));
#17362=CARTESIAN_POINT('Ctrl Pts',(5.19107814923646,2.44856947914658,11.1590608047071));
#17363=CARTESIAN_POINT('Ctrl Pts',(5.27235166789332,2.44534150031038,11.1548336034926));
#17364=CARTESIAN_POINT('Ctrl Pts',(5.35355449923363,2.43805910519284,11.1506064022781));
#17365=CARTESIAN_POINT('Ctrl Pts',(5.43425204526809,2.42673878783738,11.1463792010636));
#17366=CARTESIAN_POINT('Ctrl Pts',(5.51478326366659,2.4154418030579,11.1421607126343));
#17367=CARTESIAN_POINT('Ctrl Pts',(5.5948108139099,2.40012356453679,11.137942224205));
#17368=CARTESIAN_POINT('Ctrl Pts',(5.67390647719009,2.38085241678126,11.1337237357757));
#17369=CARTESIAN_POINT('Ctrl Pts',(5.75297620718848,2.36158758750243,11.1295066304722));
#17370=CARTESIAN_POINT('Ctrl Pts',(5.83111420586797,2.33837253274122,11.1252895251686));
#17371=CARTESIAN_POINT('Ctrl Pts',(5.90790326982822,2.31132653037253,11.1210724198651));
#17372=CARTESIAN_POINT('Ctrl Pts',(5.98469065230795,2.28428112024086,11.1168554069052));
#17373=CARTESIAN_POINT('Ctrl Pts',(6.06012872088491,2.25340508474976,11.1126383939453));
#17374=CARTESIAN_POINT('Ctrl Pts',(6.13381760662518,2.21886685302902,11.1084213809854));
#17375=CARTESIAN_POINT('Ctrl Pts',(6.20781119841862,2.18418580454337,11.1041869305332));
#17376=CARTESIAN_POINT('Ctrl Pts',(6.28004067809311,2.14581239738208,11.099952480081));
#17377=CARTESIAN_POINT('Ctrl Pts',(6.35012523456467,2.10396420749513,11.0957180296288));
#17378=CARTESIAN_POINT('Ctrl Pts',(6.42002238088403,2.06222792208515,11.0914949023417));
#17379=CARTESIAN_POINT('Ctrl Pts',(6.48778569450197,2.01703570745296,11.0872717750547));
#17380=CARTESIAN_POINT('Ctrl Pts',(6.55306722968888,1.96864640190776,11.0830486477676));
#17381=CARTESIAN_POINT('Ctrl Pts',(6.61861131684873,1.92006248225609,11.0788085357329));
#17382=CARTESIAN_POINT('Ctrl Pts',(6.68165326216365,1.86825600713603,11.0745684236981));
#17383=CARTESIAN_POINT('Ctrl Pts',(6.74187651914453,1.81352792777952,11.0703283116634));
#17384=CARTESIAN_POINT('Ctrl Pts',(6.8020997761254,1.75879984842303,11.0660881996287));
#17385=CARTESIAN_POINT('Ctrl Pts',(6.85950405911743,1.70115053986479,11.061848087594));
#17386=CARTESIAN_POINT('Ctrl Pts',(6.91381319192505,1.64091470742607,11.0576079755592));
#17387=CARTESIAN_POINT('Ctrl Pts',(6.96744889695082,1.58142579324822,11.0534204404871));
#17388=CARTESIAN_POINT('Ctrl Pts',(7.0182754860553,1.51918136673991,11.0492329054149));
#17389=CARTESIAN_POINT('Ctrl Pts',(7.06599273028175,1.45448038675701,11.0450453703427));
#17390=CARTESIAN_POINT('Ctrl Pts',(7.11364716714047,1.38986456882209,11.0408633470737));
#17391=CARTESIAN_POINT('Ctrl Pts',(7.15820009828966,1.32279898971227,11.0366813238046));
#17392=CARTESIAN_POINT('Ctrl Pts',(7.19938935247714,1.25361799782205,11.0324993005356));
#17393=CARTESIAN_POINT('Ctrl Pts',(7.24053764073229,1.18450581183491,11.0283214366155));
#17394=CARTESIAN_POINT('Ctrl Pts',(7.27832864894172,1.11328279391638,11.0241435726954));
#17395=CARTESIAN_POINT('Ctrl Pts',(7.31254255077461,1.04031353185631,11.0199657087753));
#17396=CARTESIAN_POINT('Ctrl Pts',(7.3467334246522,0.96739338237375,11.0157906568018));
#17397=CARTESIAN_POINT('Ctrl Pts',(7.37735177122243,0.892729751330217,11.0116156048283));
#17398=CARTESIAN_POINT('Ctrl Pts',(7.40422367988037,0.816711791217957,11.0074405528548));
#17399=CARTESIAN_POINT('Ctrl Pts',(7.43109295644617,0.740701277032877,11.0032659098258));
#17400=CARTESIAN_POINT('Ctrl Pts',(7.45421635323715,0.663337140612717,10.9990912667969));
#17401=CARTESIAN_POINT('Ctrl Pts',(7.47346857645307,0.585027313431843,10.994916623768));
#17402=CARTESIAN_POINT('Ctrl Pts',(7.49271959479406,0.506722387167932,10.9907422420035));
#17403=CARTESIAN_POINT('Ctrl Pts',(7.50809981523551,0.427472351205318,10.9865678602391));
#17404=CARTESIAN_POINT('Ctrl Pts',(7.51953466754609,0.347697161011841,10.9823934784747));
#17405=CARTESIAN_POINT('Ctrl Pts',(7.53097725214843,0.267868026523438,10.978216273977));
#17406=CARTESIAN_POINT('Ctrl Pts',(7.53846908540081,0.187513500945867,10.9740390694793));
#17407=CARTESIAN_POINT('Ctrl Pts',(7.54198738688373,0.107059475253671,10.9698618649817));
#17408=CARTESIAN_POINT('Ctrl Pts',(7.54357977837128,0.0706457948815983,
10.9679712524472));
#17409=CARTESIAN_POINT('Ctrl Pts',(7.54435890520214,0.0342117574601048,
10.9660806399126));
#17410=CARTESIAN_POINT('Ctrl Pts',(7.54432616501601,-0.00220320930647693,
10.9641900273781));
#17411=CARTESIAN_POINT('',(7.54432706806737,0.000654429156073597,10.1641900273412));
#17412=CARTESIAN_POINT('Ctrl Pts',(7.54432616501525,-0.00220321015041382,
10.9641900273343));
#17413=CARTESIAN_POINT('Ctrl Pts',(7.54422973877533,-0.109452355392079,
10.9586218064537));
#17414=CARTESIAN_POINT('Ctrl Pts',(7.53708802523116,-0.216389415989995,
10.9530535855732));
#17415=CARTESIAN_POINT('Ctrl Pts',(7.52304979361354,-0.32222294184132,10.9474853646926));
#17416=CARTESIAN_POINT('Ctrl Pts',(7.50901156199592,-0.428056467692646,
10.9419171438121));
#17417=CARTESIAN_POINT('Ctrl Pts',(7.48807700937725,-0.532786801160541,
10.9363489229316));
#17418=CARTESIAN_POINT('Ctrl Pts',(7.46044938521055,-0.635648858740374,
10.930780702051));
#17419=CARTESIAN_POINT('Ctrl Pts',(7.43945115546565,-0.713828622011396,
10.926548605197));
#17420=CARTESIAN_POINT('Ctrl Pts',(7.41453567237304,-0.79111260545169,10.922316508343));
#17421=CARTESIAN_POINT('Ctrl Pts',(7.38579644898933,-0.867079585440167,
10.918084411489));
#17422=CARTESIAN_POINT('Ctrl Pts',(7.35709830020516,-0.942937992095254,
10.9138583632216));
#17423=CARTESIAN_POINT('Ctrl Pts',(7.32458742817768,-1.01748270272683,10.9096323149543));
#17424=CARTESIAN_POINT('Ctrl Pts',(7.28840760300555,-1.09030587874254,10.9054062666869));
#17425=CARTESIAN_POINT('Ctrl Pts',(7.25221790407295,-1.163148928779,10.9011790650976));
#17426=CARTESIAN_POINT('Ctrl Pts',(7.21235739572926,-1.23426906122187,10.8969518635082));
#17427=CARTESIAN_POINT('Ctrl Pts',(7.16901889602631,-1.30327644414251,10.8927246619189));
#17428=CARTESIAN_POINT('Ctrl Pts',(7.12576974739914,-1.37214155439699,10.88850617556));
#17429=CARTESIAN_POINT('Ctrl Pts',(7.07905716023836,-1.43890221131252,10.884287689201));
#17430=CARTESIAN_POINT('Ctrl Pts',(7.0291186574484,-1.50319561345315,10.8800692028421));
#17431=CARTESIAN_POINT('Ctrl Pts',(6.97919653018364,-1.56746793289871,10.8758520997831));
#17432=CARTESIAN_POINT('Ctrl Pts',(6.92605087285857,-1.62927423755848,10.8716349967241));
#17433=CARTESIAN_POINT('Ctrl Pts',(6.86996118027363,-1.68828261137608,10.8674178936651));
#17434=CARTESIAN_POINT('Ctrl Pts',(6.81387271819393,-1.74728969065792,10.8632008831217));
#17435=CARTESIAN_POINT('Ctrl Pts',(6.75484067025096,-1.80349862512478,10.8589838725782));
#17436=CARTESIAN_POINT('Ctrl Pts',(6.69318229220123,-1.85661342140937,10.8547668620348));
#17437=CARTESIAN_POINT('Ctrl Pts',(6.63126888498284,-1.90994790920659,10.8505324092438));
#17438=CARTESIAN_POINT('Ctrl Pts',(6.56670772462401,-1.9601622909648,10.8462979564528));
#17439=CARTESIAN_POINT('Ctrl Pts',(6.49985312011632,-2.00699806594149,10.8420635036618));
#17440=CARTESIAN_POINT('Ctrl Pts',(6.43317736997772,-2.05370854239843,10.8378403791912));
#17441=CARTESIAN_POINT('Ctrl Pts',(6.36422084896978,-2.09705825239817,10.8336172547207));
#17442=CARTESIAN_POINT('Ctrl Pts',(6.29336207432357,-2.13683556419544,10.8293941302501));
#17443=CARTESIAN_POINT('Ctrl Pts',(6.22221818699229,-2.17677292697056,10.8251540132989));
#17444=CARTESIAN_POINT('Ctrl Pts',(6.14915713162086,-2.21310888042652,10.8209138963477));
#17445=CARTESIAN_POINT('Ctrl Pts',(6.07458301303673,-2.24567767006207,10.8166737793965));
#17446=CARTESIAN_POINT('Ctrl Pts',(6.00000889445258,-2.27824645969764,10.8124336624453));
#17447=CARTESIAN_POINT('Ctrl Pts',(5.92392217172948,-2.30704797824904,10.8081935454941));
#17448=CARTESIAN_POINT('Ctrl Pts',(5.84674123807394,-2.33196711687606,10.8039534285428));
#17449=CARTESIAN_POINT('Ctrl Pts',(5.76970641228079,-2.35683908216758,10.7997213383723));
#17450=CARTESIAN_POINT('Ctrl Pts',(5.69129412275253,-2.37793615913651,10.7954892482017));
#17451=CARTESIAN_POINT('Ctrl Pts',(5.61190875683385,-2.39510786903446,10.7912571580311));
#17452=CARTESIAN_POINT('Ctrl Pts',(5.53263685098873,-2.41225503658199,10.7870311164975));
#17453=CARTESIAN_POINT('Ctrl Pts',(5.45239508132609,-2.42548788221857,10.782805074964));
#17454=CARTESIAN_POINT('Ctrl Pts',(5.37160391926511,-2.43470538658913,10.7785790334304));
#17455=CARTESIAN_POINT('Ctrl Pts',(5.29079054782651,-2.44392542483877,10.7743518301639));
#17456=CARTESIAN_POINT('Ctrl Pts',(5.20942793358248,-2.44912779598901,10.7701246268974));
#17457=CARTESIAN_POINT('Ctrl Pts',(5.12794809816666,-2.45026243722348,10.7658974236309));
#17458=CARTESIAN_POINT('Ctrl Pts',(5.04663641333607,-2.45139473688979,10.7616789440775));
#17459=CARTESIAN_POINT('Ctrl Pts',(4.9652084549966,-2.44847604761776,10.757460464524));
#17460=CARTESIAN_POINT('Ctrl Pts',(4.88409785474619,-2.44150852352086,10.7532419849706));
#17461=CARTESIAN_POINT('Ctrl Pts',(4.80301385204959,-2.43454328419433,10.7490248887288));
#17462=CARTESIAN_POINT('Ctrl Pts',(4.72224746339989,-2.42353188643918,10.744807792487));
#17463=CARTESIAN_POINT('Ctrl Pts',(4.64222921171153,-2.40852850246958,10.7405906962452));
#17464=CARTESIAN_POINT('Ctrl Pts',(4.56221271552293,-2.39352544765536,10.7363736925211));
#17465=CARTESIAN_POINT('Ctrl Pts',(4.48294478017963,-2.37453066752338,10.7321566887971));
#17466=CARTESIAN_POINT('Ctrl Pts',(4.40484630280279,-2.35164955609488,10.7279396850731));
#17467=CARTESIAN_POINT('Ctrl Pts',(4.3264245214889,-2.32867372382601,10.7237052242365));
#17468=CARTESIAN_POINT('Ctrl Pts',(4.24918235755605,-2.3017794355617,10.7194707634));
#17469=CARTESIAN_POINT('Ctrl Pts',(4.1735293841398,-2.27112356821811,10.7152363025635));
#17470=CARTESIAN_POINT('Ctrl Pts',(4.09807906717904,-2.24054982070584,10.7110131848478));
#17471=CARTESIAN_POINT('Ctrl Pts',(4.02420984418272,-2.20623485547402,10.7067900671322));
#17472=CARTESIAN_POINT('Ctrl Pts',(3.95230510324244,-2.16838134430195,10.7025669494165));
#17473=CARTESIAN_POINT('Ctrl Pts',(3.88011066252651,-2.13037532366319,10.6983268170196));
#17474=CARTESIAN_POINT('Ctrl Pts',(3.80989696810958,-2.08880243134801,10.6940866846226));
#17475=CARTESIAN_POINT('Ctrl Pts',(3.7420228151154,-2.04391175823325,10.6898465522256));
#17476=CARTESIAN_POINT('Ctrl Pts',(3.67414866212122,-1.99902108511848,10.6856064198286));
#17477=CARTESIAN_POINT('Ctrl Pts',(3.60861439013521,-1.95081295823496,10.6813662874316));
#17478=CARTESIAN_POINT('Ctrl Pts',(3.545744050563,-1.89957599225559,10.6771261550346));
#17479=CARTESIAN_POINT('Ctrl Pts',(3.48299299799072,-1.84843624070195,10.6728940676502));
#17480=CARTESIAN_POINT('Ctrl Pts',(3.42266165538615,-1.79408835227847,10.6686619802658));
#17481=CARTESIAN_POINT('Ctrl Pts',(3.36509614527464,-1.736789954038,10.6644298928814));
#17482=CARTESIAN_POINT('Ctrl Pts',(3.30761291060314,-1.67957344946821,10.6602038542031));
#17483=CARTESIAN_POINT('Ctrl Pts',(3.25288798380879,-1.61941513560699,10.6559778155248));
#17484=CARTESIAN_POINT('Ctrl Pts',(3.20123471640633,-1.55661302502033,10.6517517768465));
#17485=CARTESIAN_POINT('Ctrl Pts',(3.1495672060652,-1.49379359729859,10.6475245728748));
#17486=CARTESIAN_POINT('Ctrl Pts',(3.1009733938187,-1.42832922967434,10.6432973689031));
#17487=CARTESIAN_POINT('Ctrl Pts',(3.05573013969367,-1.3605553293977,10.6390701649314));
#17488=CARTESIAN_POINT('Ctrl Pts',(3.01058029410279,-1.29292135408445,10.6348516883808));
#17489=CARTESIAN_POINT('Ctrl Pts',(2.9687674642413,-1.22298774567671,10.6306332118301));
#17490=CARTESIAN_POINT('Ctrl Pts',(2.93052555595295,-1.15111964608378,10.6264147352795));
#17491=CARTESIAN_POINT('Ctrl Pts',(2.89229618829429,-1.0792751141229,10.6221976420895));
#17492=CARTESIAN_POINT('Ctrl Pts',(2.85763563481092,-1.00549776069986,10.6179805488995));
#17493=CARTESIAN_POINT('Ctrl Pts',(2.82673244980861,-0.930178394523694,
10.6137634557095));
#17494=CARTESIAN_POINT('Ctrl Pts',(2.79582994311389,-0.854860681565405,
10.6095464550823));
#17495=CARTESIAN_POINT('Ctrl Pts',(2.76868481625073,-0.778001453495694,
10.6053294544552));
#17496=CARTESIAN_POINT('Ctrl Pts',(2.74543739777439,-0.700011282787416,
10.601112453828));
#17497=CARTESIAN_POINT('Ctrl Pts',(2.72209370549917,-0.621698133851823,
10.5968779894696));
#17498=CARTESIAN_POINT('Ctrl Pts',(2.70268022044022,-0.542245103709113,
10.5926435251111));
#17499=CARTESIAN_POINT('Ctrl Pts',(2.68728790353319,-0.462081247151078,
10.5884090607526));
#17500=CARTESIAN_POINT('Ctrl Pts',(2.67193684332346,-0.382132257268758,
10.5841859462133));
#17501=CARTESIAN_POINT('Ctrl Pts',(2.66058544696529,-0.3014767153737,10.5799628316741));
#17502=CARTESIAN_POINT('Ctrl Pts',(2.65327200300634,-0.220546588877568,
10.5757397171348));
#17503=CARTESIAN_POINT('Ctrl Pts',(2.64592907620976,-0.13929020709157,10.5714995778668));
#17504=CARTESIAN_POINT('Ctrl Pts',(2.64265673743915,-0.0577574935697764,
10.5672594385987));
#17505=CARTESIAN_POINT('Ctrl Pts',(2.64344094462743,0.0236149909031273,
10.5630192993306));
#17506=CARTESIAN_POINT('Ctrl Pts',(2.64422515181571,0.104987475376031,10.5587791600625));
#17507=CARTESIAN_POINT('Ctrl Pts',(2.64906581505827,0.186199267992801,10.5545390207944));
#17508=CARTESIAN_POINT('Ctrl Pts',(2.65789683120662,0.266821486047086,10.5502988815263));
#17509=CARTESIAN_POINT('Ctrl Pts',(2.66671108469566,0.347290670435662,10.5460667907103));
#17510=CARTESIAN_POINT('Ctrl Pts',(2.67953342465925,0.42747273257862,10.5418346998942));
#17511=CARTESIAN_POINT('Ctrl Pts',(2.69633575483152,0.506937110444215,10.5376026090782));
#17512=CARTESIAN_POINT('Ctrl Pts',(2.71311407052352,0.586287915030661,10.5333765669149));
#17513=CARTESIAN_POINT('Ctrl Pts',(2.73386098343242,0.664922621732558,10.5291505247517));
#17514=CARTESIAN_POINT('Ctrl Pts',(2.75849668575241,0.74241622240325,10.5249244825884));
#17515=CARTESIAN_POINT('Ctrl Pts',(2.7831391557917,0.819931111484143,10.5206972794814));
#17516=CARTESIAN_POINT('Ctrl Pts',(2.81167247496008,0.8963038070958,10.5164700763743));
#17517=CARTESIAN_POINT('Ctrl Pts',(2.84396561234774,0.971119604814727,10.5122428732672));
#17518=CARTESIAN_POINT('Ctrl Pts',(2.87619211182324,1.04578101776465,10.5080243931276));
#17519=CARTESIAN_POINT('Ctrl Pts',(2.91216276679483,1.11889151524476,10.503805912988));
#17520=CARTESIAN_POINT('Ctrl Pts',(2.95169823893658,1.19005628229245,10.4995874328485));
#17521=CARTESIAN_POINT('Ctrl Pts',(2.99122074655504,1.26119771289744,10.4953703360384));
#17522=CARTESIAN_POINT('Ctrl Pts',(3.03430552436084,1.3303942742741,10.4911532392283));
#17523=CARTESIAN_POINT('Ctrl Pts',(3.08072703822684,1.39727526565942,10.4869361424183));
#17524=CARTESIAN_POINT('Ctrl Pts',(3.12714753345736,1.46415478946331,10.4827191381447));
#17525=CARTESIAN_POINT('Ctrl Pts',(3.1769043532607,1.52871846321255,10.4785021338711));
#17526=CARTESIAN_POINT('Ctrl Pts',(3.22972916009567,1.59062532159663,10.4742851295976));
#17527=CARTESIAN_POINT('Ctrl Pts',(3.28277262981773,1.65278843709163,10.4700506694659));
#17528=CARTESIAN_POINT('Ctrl Pts',(3.33890924345049,1.71227232788743,10.4658162093343));
#17529=CARTESIAN_POINT('Ctrl Pts',(3.39782831669486,1.76876742081334,10.4615817492027));
#17530=CARTESIAN_POINT('Ctrl Pts',(3.45658957635809,1.8251111927418,10.4573586309894));
#17531=CARTESIAN_POINT('Ctrl Pts',(3.51811802895034,1.87848188195073,10.4531355127761));
#17532=CARTESIAN_POINT('Ctrl Pts',(3.58207191205862,1.92861254119879,10.4489123945629));
#17533=CARTESIAN_POINT('Ctrl Pts',(3.64628343407846,1.97894515235121,10.4446722634721));
#17534=CARTESIAN_POINT('Ctrl Pts',(3.71293957951195,2.02601130857226,10.4404321323813));
#17535=CARTESIAN_POINT('Ctrl Pts',(3.78166628772297,2.0695854916378,10.4361920012905));
#17536=CARTESIAN_POINT('Ctrl Pts',(3.85039299593399,2.11315967470334,10.4319518701997));
#17537=CARTESIAN_POINT('Ctrl Pts',(3.92118982959871,2.15324170850486,10.4277117391089));
#17538=CARTESIAN_POINT('Ctrl Pts',(3.99366087354392,2.18965394575264,10.4234716080181));
#17539=CARTESIAN_POINT('Ctrl Pts',(4.06599447518361,2.22599712670477,10.4192395183927));
#17540=CARTESIAN_POINT('Ctrl Pts',(4.14026579677943,2.25882002096268,10.4150074287673));
#17541=CARTESIAN_POINT('Ctrl Pts',(4.21609817081611,2.28791216604312,10.410775339142));
#17542=CARTESIAN_POINT('Ctrl Pts',(4.29182216232673,2.31696273151837,10.4065492981807));
#17543=CARTESIAN_POINT('Ctrl Pts',(4.36910234480826,2.34229297295076,10.4023232572195));
#17544=CARTESIAN_POINT('Ctrl Pts',(4.4475386030181,2.36373885126751,10.3980972162583));
#17545=CARTESIAN_POINT('Ctrl Pts',(4.52599643646458,2.38519062864052,10.3938700128521));
#17546=CARTESIAN_POINT('Ctrl Pts',(4.60561055333585,2.40275572018599,10.389642809446));
#17547=CARTESIAN_POINT('Ctrl Pts',(4.68596164252641,2.41631868207922,10.3854156060398));
#17548=CARTESIAN_POINT('Ctrl Pts',(4.76614689582192,2.42985365149657,10.3811971271209));
#17549=CARTESIAN_POINT('Ctrl Pts',(4.84706562833794,2.4394028926821,10.3769786482021));
#17550=CARTESIAN_POINT('Ctrl Pts',(4.92828896477675,2.44490232063115,10.3727601692833));
#17551=CARTESIAN_POINT('Ctrl Pts',(5.00948566626339,2.45039994519454,10.3685430736982));
#17552=CARTESIAN_POINT('Ctrl Pts',(5.09098631003848,2.4518503624904,10.3643259781131));
#17553=CARTESIAN_POINT('Ctrl Pts',(5.17235715006545,2.44924137029126,10.360108882528));
#17554=CARTESIAN_POINT('Ctrl Pts',(5.2537262045067,2.44663243534332,10.3558918794821));
#17555=CARTESIAN_POINT('Ctrl Pts',(5.33496499644998,2.43996428405307,10.3516748764361));
#17556=CARTESIAN_POINT('Ctrl Pts',(5.41564147139757,2.42927680515276,10.3474578733902));
#17557=CARTESIAN_POINT('Ctrl Pts',(5.49665194953007,2.41854507974821,10.3432234118168));
#17558=CARTESIAN_POINT('Ctrl Pts',(5.57709497531964,2.40376072474435,10.3389889502435));
#17559=CARTESIAN_POINT('Ctrl Pts',(5.65654182378683,2.38501623727011,10.3347544886701));
#17560=CARTESIAN_POINT('Ctrl Pts',(5.73577582553562,2.36632196830955,10.3305313716783));
#17561=CARTESIAN_POINT('Ctrl Pts',(5.81401854315967,2.34368892850853,10.3263082546865));
#17562=CARTESIAN_POINT('Ctrl Pts',(5.89086013740065,2.31725887109917,10.3220851376947));
#17563=CARTESIAN_POINT('Ctrl Pts',(5.96801136161381,2.29072231488509,10.3178450038305));
#17564=CARTESIAN_POINT('Ctrl Pts',(6.04374971268874,2.26035826005573,10.3136048699664));
#17565=CARTESIAN_POINT('Ctrl Pts',(6.11768256731956,2.22635809015346,10.3093647361023));
#17566=CARTESIAN_POINT('Ctrl Pts',(6.19161542195039,2.19235792025119,10.3051246022382));
#17567=CARTESIAN_POINT('Ctrl Pts',(6.26374239459648,2.15472190661922,10.3008844683741));
#17568=CARTESIAN_POINT('Ctrl Pts',(6.33369916316996,2.11368579842894,10.29664433451));
#17569=CARTESIAN_POINT('Ctrl Pts',(6.40352320773505,2.07272754513217,10.2924122451507));
#17570=CARTESIAN_POINT('Ctrl Pts',(6.47144578305982,2.02822929369221,10.2881801557914));
#17571=CARTESIAN_POINT('Ctrl Pts',(6.53708548682375,1.98039279915102,10.2839480664321));
#17572=CARTESIAN_POINT('Ctrl Pts',(6.60263137568237,1.9326246744523,10.2797220257452));
#17573=CARTESIAN_POINT('Ctrl Pts',(6.66590050079519,1.88152805407527,10.2754959850582));
#17574=CARTESIAN_POINT('Ctrl Pts',(6.72653767991026,1.82734960894921,10.2712699443713));
#17575=CARTESIAN_POINT('Ctrl Pts',(6.78719154322635,1.77315625673015,10.2670427408976));
#17576=CARTESIAN_POINT('Ctrl Pts',(6.84521162343385,1.71587964234996,10.2628155374239));
#17577=CARTESIAN_POINT('Ctrl Pts',(6.90027309244994,1.65580896443631,10.2585883339501));
#17578=CARTESIAN_POINT('Ctrl Pts',(6.95522091590697,1.59586227096944,10.2543698553236));
#17579=CARTESIAN_POINT('Ctrl Pts',(7.00722199653962,1.53313336189751,10.250151376697));
#17580=CARTESIAN_POINT('Ctrl Pts',(7.05598941581168,1.46794738121793,10.2459328980704));
#17581=CARTESIAN_POINT('Ctrl Pts',(7.10474084308195,1.40278277657864,10.2417158027838));
#17582=CARTESIAN_POINT('Ctrl Pts',(7.1502604366871,1.33516307224067,10.2374987074971));
#17583=CARTESIAN_POINT('Ctrl Pts',(7.19230217861376,1.26544570297225,10.2332816122105));
#17584=CARTESIAN_POINT('Ctrl Pts',(7.23434299792718,1.19572986366344,10.2290646094687));
#17585=CARTESIAN_POINT('Ctrl Pts',(7.27290587832797,1.12391684947886,10.224847606727));
#17586=CARTESIAN_POINT('Ctrl Pts',(7.30778944419396,1.05039099102828,10.2206306039852));
#17587=CARTESIAN_POINT('Ctrl Pts',(7.34281743449282,0.97656072188617,10.2163961420699));
#17588=CARTESIAN_POINT('Ctrl Pts',(7.37413536539507,0.901003816020216,10.2121616801546));
#17589=CARTESIAN_POINT('Ctrl Pts',(7.40158782829095,0.82413040649102,10.2079272182393));
#17590=CARTESIAN_POINT('Ctrl Pts',(7.42896673880807,0.747462961073511,10.2037041015628));
#17591=CARTESIAN_POINT('Ctrl Pts',(7.45250077239823,0.669486517032942,10.1994809848863));
#17592=CARTESIAN_POINT('Ctrl Pts',(7.47208612989054,0.590622130052558,10.1952578682098));
#17593=CARTESIAN_POINT('Ctrl Pts',(7.49175041033514,0.51143994390748,10.1910177336751));
#17594=CARTESIAN_POINT('Ctrl Pts',(7.50743404144642,0.431363107756696,10.1867775991404));
#17595=CARTESIAN_POINT('Ctrl Pts',(7.51908423982532,0.350825205340769,10.1825374646058));
#17596=CARTESIAN_POINT('Ctrl Pts',(7.53073443820423,0.270287302924853,10.1782973300711));
#17597=CARTESIAN_POINT('Ctrl Pts',(7.5383512220321,0.189288805347542,10.1740571955364));
#17598=CARTESIAN_POINT('Ctrl Pts',(7.5419344305523,0.108263657828534,10.1698170610017));
#17599=CARTESIAN_POINT('Ctrl Pts',(7.54351950878181,0.0724211449937457,
10.1679413831272));
#17600=CARTESIAN_POINT('Ctrl Pts',(7.54431748352344,0.0365435678285603,
10.1660657052527));
#17601=CARTESIAN_POINT('Ctrl Pts',(7.54432706806718,0.000654429861452634,
10.1641900273781));
#17602=CARTESIAN_POINT('',(7.54432654498802,0.00172970778312925,9.36419005773998));
#17603=CARTESIAN_POINT('Ctrl Pts',(7.54432706806737,0.000654429156057273,
10.1641900273412));
#17604=CARTESIAN_POINT('Ctrl Pts',(7.54434854189879,-0.0797540024219345,
10.1599876328403));
#17605=CARTESIAN_POINT('Ctrl Pts',(7.5404080790334,-0.160320975644378,10.1557852383394));
#17606=CARTESIAN_POINT('Ctrl Pts',(7.53248499309329,-0.240620449912523,
10.1515828438385));
#17607=CARTESIAN_POINT('Ctrl Pts',(7.52457302027542,-0.320807294091884,
10.1473863437232));
#17608=CARTESIAN_POINT('Ctrl Pts',(7.51268956108762,-0.400726918673235,
10.1431898436079));
#17609=CARTESIAN_POINT('Ctrl Pts',(7.4968659434941,-0.479952948913191,10.1389933434927));
#17610=CARTESIAN_POINT('Ctrl Pts',(7.4810596902607,-0.559092038900001,10.1348014484899));
#17611=CARTESIAN_POINT('Ctrl Pts',(7.46132196055936,-0.637538586265839,
10.1306095534871));
#17612=CARTESIAN_POINT('Ctrl Pts',(7.43773574775956,-0.714872548718988,
10.1264176584843));
#17613=CARTESIAN_POINT('Ctrl Pts',(7.41416339532711,-0.792161066100588,
10.1222282268361));
#17614=CARTESIAN_POINT('Ctrl Pts',(7.38674718491712,-0.86833784573309,10.1180387951878));
#17615=CARTESIAN_POINT('Ctrl Pts',(7.35562063746299,-0.942995490306101,
10.1138493635396));
#17616=CARTESIAN_POINT('Ctrl Pts',(7.32450251973879,-1.01763291600382,10.1096610664784));
#17617=CARTESIAN_POINT('Ctrl Pts',(7.28967624166735,-1.09075158826702,10.1054727694172));
#17618=CARTESIAN_POINT('Ctrl Pts',(7.25132384904031,-1.16196310920799,10.101284472356));
#17619=CARTESIAN_POINT('Ctrl Pts',(7.21296969209431,-1.23317790608111,10.0970959826212));
#17620=CARTESIAN_POINT('Ctrl Pts',(7.17108932405904,-1.30248496297156,10.0929074928865));
#17621=CARTESIAN_POINT('Ctrl Pts',(7.12591049597306,-1.36952091885494,10.0887190031517));
#17622=CARTESIAN_POINT('Ctrl Pts',(7.08068583939756,-1.43662487465625,10.0845262646977));
#17623=CARTESIAN_POINT('Ctrl Pts',(7.03215630761541,-1.50145273844476,10.0803335262436));
#17624=CARTESIAN_POINT('Ctrl Pts',(6.98059231048667,-1.56367116100259,10.0761407877896));
#17625=CARTESIAN_POINT('Ctrl Pts',(6.92900025391363,-1.6259234407953,10.0719457677841));
#17626=CARTESIAN_POINT('Ctrl Pts',(6.87437076456973,-1.68556310551769,10.0677507477787));
#17627=CARTESIAN_POINT('Ctrl Pts',(6.81701204751294,-1.74229276465718,10.0635557277732));
#17628=CARTESIAN_POINT('Ctrl Pts',(6.75955608575016,-1.79911860201171,10.0593535956232));
#17629=CARTESIAN_POINT('Ctrl Pts',(6.69936201018658,-1.85302426969885,10.0551514634732));
#17630=CARTESIAN_POINT('Ctrl Pts',(6.63677172159038,-1.90375216764879,10.0509493313232));
#17631=CARTESIAN_POINT('Ctrl Pts',(6.59725288308932,-1.93578121962386,10.0482961500466));
#17632=CARTESIAN_POINT('Ctrl Pts',(6.55677941399393,-1.96654429046505,10.0456429687701));
#17633=CARTESIAN_POINT('Ctrl Pts',(6.51544287596879,-1.99598571968405,10.0429897874936));
#17634=CARTESIAN_POINT('Ctrl Pts',(6.44950696129102,-2.04294774547818,10.0387576978549));
#17635=CARTESIAN_POINT('Ctrl Pts',(6.38111851702476,-2.08672664771397,10.0345256082162));
#17636=CARTESIAN_POINT('Ctrl Pts',(6.31061765686637,-2.12705691641537,10.0302935185776));
#17637=CARTESIAN_POINT('Ctrl Pts',(6.24021755927349,-2.1673295435315,10.0260674776057));
#17638=CARTESIAN_POINT('Ctrl Pts',(6.16771144212542,-2.20416309767322,10.0218414366338));
#17639=CARTESIAN_POINT('Ctrl Pts',(6.09346968053859,-2.23733436750986,10.0176153956619));
#17640=CARTESIAN_POINT('Ctrl Pts',(6.01920749772374,-2.27051476156514,10.0133881922587));
#17641=CARTESIAN_POINT('Ctrl Pts',(5.94320911055227,-2.30003060757941,10.0091609888555));
#17642=CARTESIAN_POINT('Ctrl Pts',(5.86587128518421,-2.32570378847947,10.0049337854523));
#17643=CARTESIAN_POINT('Ctrl Pts',(5.78869307653,-2.35132398277498,10.0007153065292));
#17644=CARTESIAN_POINT('Ctrl Pts',(5.71018138623775,-2.37311718764668,9.99649682760604));
#17645=CARTESIAN_POINT('Ctrl Pts',(5.63075027478033,-2.39095458215582,9.99227834868292));
#17646=CARTESIAN_POINT('Ctrl Pts',(5.55134521061032,-2.40878612737326,9.98806125309601));
#17647=CARTESIAN_POINT('Ctrl Pts',(5.47102177707208,-2.42266433661333,9.98384415750909));
#17648=CARTESIAN_POINT('Ctrl Pts',(5.39020677054033,-2.43251091955632,9.97962706192218));
#17649=CARTESIAN_POINT('Ctrl Pts',(5.30939353744409,-2.44235728642212,9.97541005887684));
#17650=CARTESIAN_POINT('Ctrl Pts',(5.22808921421871,-2.44817214783398,9.97119305583149));
#17651=CARTESIAN_POINT('Ctrl Pts',(5.14672687960594,-2.44992895186464,9.96697605278615));
#17652=CARTESIAN_POINT('Ctrl Pts',(5.06502770244309,-2.45169302911763,9.96274159121941));
#17653=CARTESIAN_POINT('Ctrl Pts',(4.98327050394719,-2.44936535339008,9.95850712965267));
#17654=CARTESIAN_POINT('Ctrl Pts',(4.90189310546524,-2.44297187262876,9.95427266808593));
#17655=CARTESIAN_POINT('Ctrl Pts',(4.82073372585589,-2.4365955206955,9.95004955110078));
#17656=CARTESIAN_POINT('Ctrl Pts',(4.73995257227418,-2.4261752220265,9.94582643411564));
#17657=CARTESIAN_POINT('Ctrl Pts',(4.65997632301412,-2.41178848682715,9.94160331713049));
#17658=CARTESIAN_POINT('Ctrl Pts',(4.57967781281918,-2.39734378088301,9.93736318327295));
#17659=CARTESIAN_POINT('Ctrl Pts',(4.50019116459454,-2.37890072070671,9.93312304941542));
#17660=CARTESIAN_POINT('Ctrl Pts',(4.4219336209088,-2.35658849361477,9.92888291555789));
#17661=CARTESIAN_POINT('Ctrl Pts',(4.34367607722305,-2.33427626652284,9.92464278170035));
#17662=CARTESIAN_POINT('Ctrl Pts',(4.26664806052866,-2.30809508180606,9.92040264784281));
#17663=CARTESIAN_POINT('Ctrl Pts',(4.19124561850282,-2.27822229362203,9.91616251398528));
#17664=CARTESIAN_POINT('Ctrl Pts',(4.11598622740603,-2.24840617906805,9.91193042436439));
#17665=CARTESIAN_POINT('Ctrl Pts',(4.04206546527135,-2.21480123235798,9.90769833474351));
#17666=CARTESIAN_POINT('Ctrl Pts',(3.9698910689718,-2.17754860416595,9.90346624512263));
#17667=CARTESIAN_POINT('Ctrl Pts',(3.8978198271362,-2.14034921888399,9.89924020416939));
#17668=CARTESIAN_POINT('Ctrl Pts',(3.82749040333833,-2.09951271786708,9.89501416321616));
#17669=CARTESIAN_POINT('Ctrl Pts',(3.75929148031584,-2.05522864464903,9.89078812226293));
#17670=CARTESIAN_POINT('Ctrl Pts',(3.69107379785709,-2.01093239023792,9.88656091885518));
#17671=CARTESIAN_POINT('Ctrl Pts',(3.62498821191902,-1.96318686309364,9.88233371544744));
#17672=CARTESIAN_POINT('Ctrl Pts',(3.56139990073167,-1.91222827062747,9.8781065120397));
#17673=CARTESIAN_POINT('Ctrl Pts',(3.49794282916259,-1.86137485136212,9.87388803313731));
#17674=CARTESIAN_POINT('Ctrl Pts',(3.43697311268567,-1.80732188749472,9.86966955423492));
#17675=CARTESIAN_POINT('Ctrl Pts',(3.37882395332888,-1.75034689896135,9.86545107533253));
#17676=CARTESIAN_POINT('Ctrl Pts',(3.32069386242832,-1.69339059384641,9.86123397976709));
#17677=CARTESIAN_POINT('Ctrl Pts',(3.26538282349114,-1.6335144919276,9.85701688420164));
#17678=CARTESIAN_POINT('Ctrl Pts',(3.21318854831214,-1.5710342705781,9.8527997886362));
#17679=CARTESIAN_POINT('Ctrl Pts',(3.16099541851314,-1.50855542032909,9.84858278561303));
#17680=CARTESIAN_POINT('Ctrl Pts',(3.1119192135165,-1.44347292163379,9.84436578258986));
#17681=CARTESIAN_POINT('Ctrl Pts',(3.06621763311378,-1.37613584900578,9.84014877956669));
#17682=CARTESIAN_POINT('Ctrl Pts',(3.0203268462704,-1.30851999810087,9.83591431797588));
#17683=CARTESIAN_POINT('Ctrl Pts',(2.97783896132303,-1.23863124858803,9.83167985638508));
#17684=CARTESIAN_POINT('Ctrl Pts',(2.93897018992724,-1.16685119365095,9.82744539479428));
#17685=CARTESIAN_POINT('Ctrl Pts',(2.9002055526215,-1.09526344607108,9.82322227783283));
#17686=CARTESIAN_POINT('Ctrl Pts',(2.86504082628364,-1.02179495372241,9.81899916087137));
#17687=CARTESIAN_POINT('Ctrl Pts',(2.83364288627533,-0.94684598502676,9.81477604390992));
#17688=CARTESIAN_POINT('Ctrl Pts',(2.80211842905418,-0.871595011338996,
9.81053591000444));
#17689=CARTESIAN_POINT('Ctrl Pts',(2.77439133067801,-0.794852051357482,
9.80629577609897));
#17690=CARTESIAN_POINT('Ctrl Pts',(2.75057996189576,-0.71703754426502,9.80205564219349));
#17691=CARTESIAN_POINT('Ctrl Pts',(2.72676859311351,-0.639223037172568,
9.79781550828802));
#17692=CARTESIAN_POINT('Ctrl Pts',(2.70687300789252,-0.56033745132404,9.79357537438254));
#17693=CARTESIAN_POINT('Ctrl Pts',(2.69095962667345,-0.480809618389983,
9.78933524047707));
#17694=CARTESIAN_POINT('Ctrl Pts',(2.67507643571004,-0.401432662606144,
9.78510315079078));
#17695=CARTESIAN_POINT('Ctrl Pts',(2.66310108021354,-0.32111975827553,9.7808710611045));
#17696=CARTESIAN_POINT('Ctrl Pts',(2.65513672227462,-0.240289868957742,
9.77663897141822));
#17697=CARTESIAN_POINT('Ctrl Pts',(2.64718374730463,-0.159575504849292,
9.77241293039847));
#17698=CARTESIAN_POINT('Ctrl Pts',(2.64323042936645,-0.0783460818642417,
9.76818688937873));
#17699=CARTESIAN_POINT('Ctrl Pts',(2.64332895420887,0.00296912423532622,
9.76396084835899));
#17700=CARTESIAN_POINT('Ctrl Pts',(2.64342750615052,0.0843066960617253,
9.75973364496773));
#17701=CARTESIAN_POINT('Ctrl Pts',(2.64758019548308,0.165729635975825,9.75550644157648));
#17702=CARTESIAN_POINT('Ctrl Pts',(2.655787263711,0.246803031330851,9.75127923818523));
#17703=CARTESIAN_POINT('Ctrl Pts',(2.66397739357458,0.327709101318281,9.74706075921409));
#17704=CARTESIAN_POINT('Ctrl Pts',(2.67620516165238,0.408266603264365,9.74284228024295));
#17705=CARTESIAN_POINT('Ctrl Pts',(2.69241875184998,0.488045007252681,9.73862380127181));
#17706=CARTESIAN_POINT('Ctrl Pts',(2.70862702523854,0.567797250067942,9.73440670563693));
#17707=CARTESIAN_POINT('Ctrl Pts',(2.72881843260256,0.646770447266115,9.73018961000204));
#17708=CARTESIAN_POINT('Ctrl Pts',(2.75288983833351,0.724543116258019,9.72597251436715));
#17709=CARTESIAN_POINT('Ctrl Pts',(2.77696071583163,0.802314078574487,9.72175551127394));
#17710=CARTESIAN_POINT('Ctrl Pts',(2.80491128391425,0.878884121492782,9.71753850818074));
#17711=CARTESIAN_POINT('Ctrl Pts',(2.83658862509982,0.953847192735038,9.71332150508754));
#17712=CARTESIAN_POINT('Ctrl Pts',(2.86839711065726,1.02912061151669,9.70908704357765));
#17713=CARTESIAN_POINT('Ctrl Pts',(2.9039631209882,1.10277328492846,9.70485258206775));
#17714=CARTESIAN_POINT('Ctrl Pts',(2.94308389171338,1.17441630756651,9.70061812055787));
#17715=CARTESIAN_POINT('Ctrl Pts',(2.98209985461162,1.2458673925362,9.69639500352563));
#17716=CARTESIAN_POINT('Ctrl Pts',(3.02465127584591,1.31531920384112,9.69217188649339));
#17717=CARTESIAN_POINT('Ctrl Pts',(3.07049289756892,1.38241409529569,9.68794876946115));
#17718=CARTESIAN_POINT('Ctrl Pts',(3.11651923448535,1.44977934031515,9.68370863571243));
#17719=CARTESIAN_POINT('Ctrl Pts',(3.16586205111719,1.51476826107213,9.67946850196373));
#17720=CARTESIAN_POINT('Ctrl Pts',(3.21823279302563,1.57705295967836,9.67522836821501));
#17721=CARTESIAN_POINT('Ctrl Pts',(3.27060353493407,1.63933765828457,9.6709882344663));
#17722=CARTESIAN_POINT('Ctrl Pts',(3.32600183833794,1.69891783485359,9.66674810071759));
#17723=CARTESIAN_POINT('Ctrl Pts',(3.38410386532814,1.75550463434428,9.66250796696887));
#17724=CARTESIAN_POINT('Ctrl Pts',(3.44209566508421,1.81198408118793,9.658275877315));
#17725=CARTESIAN_POINT('Ctrl Pts',(3.50299728362813,1.8656922229589,9.65404378766113));
#17726=CARTESIAN_POINT('Ctrl Pts',(3.56651313793106,1.91631472933875,9.64981169800726));
#17727=CARTESIAN_POINT('Ctrl Pts',(3.62993821290765,1.96686488406598,9.64558565702032));
#17728=CARTESIAN_POINT('Ctrl Pts',(3.69596974245763,2.01433787515468,9.64135961603339));
#17729=CARTESIAN_POINT('Ctrl Pts',(3.76427577817759,2.0584565541164,9.63713357504646));
#17730=CARTESIAN_POINT('Ctrl Pts',(3.83260060211758,2.10258736833731,9.63290637164705));
#17731=CARTESIAN_POINT('Ctrl Pts',(3.90320083122195,2.14336171876855,9.62867916824763));
#17732=CARTESIAN_POINT('Ctrl Pts',(3.97571154982909,2.18054299257319,9.62445196484822));
#17733=CARTESIAN_POINT('Ctrl Pts',(4.04807261465002,2.21764752850365,9.6202334859106));
#17734=CARTESIAN_POINT('Ctrl Pts',(4.12233588867171,2.25117357010085,9.61601500697299));
#17735=CARTESIAN_POINT('Ctrl Pts',(4.19811183741161,2.28093058180774,9.61179652803537));
#17736=CARTESIAN_POINT('Ctrl Pts',(4.27386293747197,2.31067783550486,9.60757943243419));
#17737=CARTESIAN_POINT('Ctrl Pts',(4.35112529495952,2.33665834407588,9.60336233683301));
#17738=CARTESIAN_POINT('Ctrl Pts',(4.42948907303053,2.35872956530483,9.59914524123183));
#17739=CARTESIAN_POINT('Ctrl Pts',(4.5078511314518,2.38080030219303,9.59492823817248));
#17740=CARTESIAN_POINT('Ctrl Pts',(4.58731411480222,2.39896179743436,9.59071123511313));
#17741=CARTESIAN_POINT('Ctrl Pts',(4.66745407731082,2.41312168119129,9.58649423205378));
#17742=CARTESIAN_POINT('Ctrl Pts',(4.74792582111546,2.42734018719407,9.58225977050435));
#17743=CARTESIAN_POINT('Ctrl Pts',(4.82907969907151,2.43752378283135,9.57802530895492));
#17744=CARTESIAN_POINT('Ctrl Pts',(4.91047906192067,2.4436312583117,9.57379084740549));
#17745=CARTESIAN_POINT('Ctrl Pts',(4.9916603476385,2.44972237124711,9.56956773040712));
#17746=CARTESIAN_POINT('Ctrl Pts',(5.07308533611265,2.451759206279,9.56534461340874));
#17747=CARTESIAN_POINT('Ctrl Pts',(5.15432051711923,2.44975321271232,9.56112149641036));
#17748=CARTESIAN_POINT('Ctrl Pts',(5.23588303099101,2.44773913610067,9.55688136258541));
#17749=CARTESIAN_POINT('Ctrl Pts',(5.31725373503828,2.44164962516437,9.55264122876045));
#17750=CARTESIAN_POINT('Ctrl Pts',(5.39800055325116,2.43154864110755,9.5484010949355));
#17751=CARTESIAN_POINT('Ctrl Pts',(5.47874737146404,2.42144765705074,9.54416096111054));
#17752=CARTESIAN_POINT('Ctrl Pts',(5.55886985438629,2.4073353422032,9.53992082728559));
#17753=CARTESIAN_POINT('Ctrl Pts',(5.63794951747986,2.38932649613702,9.53568069346063));
#17754=CARTESIAN_POINT('Ctrl Pts',(5.71687915457687,2.37135181555629,9.5314486038063));
#17755=CARTESIAN_POINT('Ctrl Pts',(5.79506439894742,2.34942833051714,9.52721651415196));
#17756=CARTESIAN_POINT('Ctrl Pts',(5.87208074203687,2.32363327678218,9.52298442449763));
#17757=CARTESIAN_POINT('Ctrl Pts',(5.94898701037536,2.29787509034061,9.51875838351032));
#17758=CARTESIAN_POINT('Ctrl Pts',(6.02472725855453,2.26825647147654,9.51453234252301));
#17759=CARTESIAN_POINT('Ctrl Pts',(6.09888841932976,2.23490539080621,9.5103063015357));
#17760=CARTESIAN_POINT('Ctrl Pts',(6.173069978824,2.20154513661007,9.5060790981364));
#17761=CARTESIAN_POINT('Ctrl Pts',(6.24567113357773,2.16445049642907,9.50185189473709));
#17762=CARTESIAN_POINT('Ctrl Pts',(6.31629491986031,2.12379914657325,9.49762469133779));
#17763=CARTESIAN_POINT('Ctrl Pts',(6.38677294677289,2.08323169642682,9.49340621239999));
#17764=CARTESIAN_POINT('Ctrl Pts',(6.45528134395035,2.03912241338701,9.48918773346218));
#17765=CARTESIAN_POINT('Ctrl Pts',(6.5214484406292,1.99169468446149,9.48496925452438));
#17766=CARTESIAN_POINT('Ctrl Pts',(6.58759383959105,1.94428250818211,9.48075215892311));
#17767=CARTESIAN_POINT('Ctrl Pts',(6.65139908537499,1.89355431758388,9.47653506332184));
#17768=CARTESIAN_POINT('Ctrl Pts',(6.71252175478821,1.83977662885563,9.47231796772057));
#17769=CARTESIAN_POINT('Ctrl Pts',(6.77364308289735,1.7860001202498,9.4681009646612));
#17770=CARTESIAN_POINT('Ctrl Pts',(6.83208160356233,1.72917455438392,9.46388396160181));
#17771=CARTESIAN_POINT('Ctrl Pts',(6.88752933678227,1.66960556260902,9.45966695854244));
#17772=CARTESIAN_POINT('Ctrl Pts',(6.94320662489477,1.60978995383625,9.45543249699327));
#17773=CARTESIAN_POINT('Ctrl Pts',(6.99586797807153,1.54720849164653,9.45119803544411));
#17774=CARTESIAN_POINT('Ctrl Pts',(7.04524145247934,1.48220527976446,9.44696357389494));
#17775=CARTESIAN_POINT('Ctrl Pts',(7.09448265035309,1.41737621806471,9.44274045689675));
#17776=CARTESIAN_POINT('Ctrl Pts',(7.14045333416895,1.35013877554875,9.43851733989857));
#17777=CARTESIAN_POINT('Ctrl Pts',(7.18292746618856,1.28086304563956,9.43429422290038));
#17778=CARTESIAN_POINT('Ctrl Pts',(7.2255727454755,1.21130817284262,9.43005408907572));
#17779=CARTESIAN_POINT('Ctrl Pts',(7.26469301668231,1.13969896950125,9.42581395525107));
#17780=CARTESIAN_POINT('Ctrl Pts',(7.30010709790708,1.06643286967595,9.42157382142642));
#17781=CARTESIAN_POINT('Ctrl Pts',(7.33552117913186,0.993166769850654,9.41733368760177));
#17782=CARTESIAN_POINT('Ctrl Pts',(7.36722894552435,0.91824422816336,9.41309355377711));
#17783=CARTESIAN_POINT('Ctrl Pts',(7.39509927477985,0.842078905334526,9.40885341995246));
#17784=CARTESIAN_POINT('Ctrl Pts',(7.42717646113868,0.754416889142964,9.40397326365316));
#17785=CARTESIAN_POINT('Ctrl Pts',(7.45427036000665,0.664839421432015,9.39909310735387));
#17786=CARTESIAN_POINT('Ctrl Pts',(7.47618097156191,0.573881995598245,9.39421295105457));
#17787=CARTESIAN_POINT('Ctrl Pts',(7.49864678047041,0.480619781422444,9.38920913550214));
#17788=CARTESIAN_POINT('Ctrl Pts',(7.51566290806526,0.385906846858317,9.3842053199497));
#17789=CARTESIAN_POINT('Ctrl Pts',(7.52706584652707,0.290344144526261,9.37920150439727));
#17790=CARTESIAN_POINT('Ctrl Pts',(7.53846878498888,0.194781442194193,9.37419768884484));
#17791=CARTESIAN_POINT('Ctrl Pts',(7.54425833113838,0.0983691508998505,
9.36919387329241));
#17792=CARTESIAN_POINT('Ctrl Pts',(7.54432654498802,0.00172970778312925,
9.36419005773998));
#17793=CARTESIAN_POINT('',(7.54193256524886,-0.00182552700443595,8.56419002737812));
#17794=CARTESIAN_POINT('Ctrl Pts',(7.54171142860237,0.00172727612123974,
9.36419002737812));
#17795=CARTESIAN_POINT('Ctrl Pts',(7.538260521488,-0.526658746908139,9.33680206706682));
#17796=CARTESIAN_POINT('Ctrl Pts',(7.11114849623935,-1.87574082982533,9.26713834891945));
#17797=CARTESIAN_POINT('Ctrl Pts',(4.88956789508618,-2.88771068875909,9.15519887293596));
#17798=CARTESIAN_POINT('Ctrl Pts',(2.55897584314901,-1.39825737663462,9.02837159942777));
#17799=CARTESIAN_POINT('Ctrl Pts',(2.54229391302319,1.36757924066726,8.9015443259196));
#17800=CARTESIAN_POINT('Ctrl Pts',(4.85475001434308,2.88503673937529,8.77471705241131));
#17801=CARTESIAN_POINT('Ctrl Pts',(7.09859130083223,1.89543275086705,8.66226561956423));
#17802=CARTESIAN_POINT('Ctrl Pts',(7.53819517521869,0.536315141057368,8.59208994455313));
#17803=CARTESIAN_POINT('Ctrl Pts',(7.54193256524886,-0.00182552700443595,
8.56419002737812));
#17804=CARTESIAN_POINT('',(7.54820287115862,-0.000480549575520677,7.76419002737812));
#17805=CARTESIAN_POINT('Ctrl Pts',(7.54193256524886,-0.00182552700443595,
8.56419002737812));
#17806=CARTESIAN_POINT('Ctrl Pts',(7.54385831016147,-0.27911038232396,8.54981418671706));
#17807=CARTESIAN_POINT('Ctrl Pts',(7.37249801786638,-1.36951156998236,8.49316258821991));
#17808=CARTESIAN_POINT('Ctrl Pts',(5.77063350138978,-2.81469856946862,8.3942352318867));
#17809=CARTESIAN_POINT('Ctrl Pts',(3.09918932920222,-2.09809790261087,8.26740795837852));
#17810=CARTESIAN_POINT('Ctrl Pts',(2.24852755674676,0.533727515180221,8.14058068487021));
#17811=CARTESIAN_POINT('Ctrl Pts',(3.99516508500167,2.67834585552468,8.01375341136209));
#17812=CARTESIAN_POINT('Ctrl Pts',(6.71513911122288,2.38129549316238,7.88828985886462));
#17813=CARTESIAN_POINT('Ctrl Pts',(7.546090913882,0.783450873209182,7.80510206420335));
#17814=CARTESIAN_POINT('Ctrl Pts',(7.54820287115862,-0.000480549575520677,
7.76419002737812));
#17815=CARTESIAN_POINT('',(7.54432619069004,0.00217446611858361,6.96419002737812));
#17816=CARTESIAN_POINT('Ctrl Pts',(7.54820287115862,-0.000480549575520677,
7.76419002737812));
#17817=CARTESIAN_POINT('Ctrl Pts',(7.54827326903503,-0.026611337364743,
7.76282630636728));
#17818=CARTESIAN_POINT('Ctrl Pts',(7.53607095936906,-0.862736996768992,
7.71918682752067));
#17819=CARTESIAN_POINT('Ctrl Pts',(6.58857747519914,-2.47917654645346,7.63327159083716));
#17820=CARTESIAN_POINT('Ctrl Pts',(3.8254306157284,-2.60226153275734,7.50644431732927));
#17821=CARTESIAN_POINT('Ctrl Pts',(2.22012507713375,-0.349901746089773,
7.37961704382094));
#17822=CARTESIAN_POINT('Ctrl Pts',(3.23804571895806,2.22186186042716,7.25278977031274));
#17823=CARTESIAN_POINT('Ctrl Pts',(5.94999528816588,2.76542419809011,7.12596249680452));
#17824=CARTESIAN_POINT('Ctrl Pts',(7.41422767974903,1.26294973299729,7.02976274506699));
#17825=CARTESIAN_POINT('Ctrl Pts',(7.54523659556225,0.226539321624495,6.97583875116552));
#17826=CARTESIAN_POINT('Ctrl Pts',(7.54330299861202,0.00218295211155193,
6.96419051510012));
#17827=CARTESIAN_POINT('',(7.54432692296551,-0.00106743696241274,6.16419002733055));
#17828=CARTESIAN_POINT('Ctrl Pts',(7.54432619069003,0.00217446611858361,
6.96419002737812));
#17829=CARTESIAN_POINT('Ctrl Pts',(7.54439769743544,-0.0784095490258181,
6.9600079418362));
#17830=CARTESIAN_POINT('Ctrl Pts',(7.54048996103695,-0.159079511651253,
6.95582585629429));
#17831=CARTESIAN_POINT('Ctrl Pts',(7.53260427432529,-0.239408467823362,
6.95164377075237));
#17832=CARTESIAN_POINT('Ctrl Pts',(7.52472246292544,-0.319697947439344,
6.94746374043864));
#17833=CARTESIAN_POINT('Ctrl Pts',(7.51286662670644,-0.399646282378628,
6.9432837101249));
#17834=CARTESIAN_POINT('Ctrl Pts',(7.49709007549609,-0.478829392525642,
6.93910367981117));
#17835=CARTESIAN_POINT('Ctrl Pts',(7.48131623537896,-0.557998895592756,
6.93492436780727));
#17836=CARTESIAN_POINT('Ctrl Pts',(7.46162311120077,-0.63640297047287,6.93074505580337));
#17837=CARTESIAN_POINT('Ctrl Pts',(7.43811525099532,-0.713627056030715,
6.92656574379946));
#17838=CARTESIAN_POINT('Ctrl Pts',(7.41460391741899,-0.790862551724909,
6.92238581428718));
#17839=CARTESIAN_POINT('Ctrl Pts',(7.38727686924611,-0.866917259459429,
6.91820588477491));
#17840=CARTESIAN_POINT('Ctrl Pts',(7.35628824494099,-0.94139262189232,6.91402595526263));
#17841=CARTESIAN_POINT('Ctrl Pts',(7.32526596372123,-1.01594887242441,6.909841485906));
#17842=CARTESIAN_POINT('Ctrl Pts',(7.29057435498374,-1.08892191757205,6.90565701654937));
#17843=CARTESIAN_POINT('Ctrl Pts',(7.25241504782298,-1.15993472269529,6.90147254719275));
#17844=CARTESIAN_POINT('Ctrl Pts',(7.214231326336,-1.23099296181404,6.89728540061246));
#17845=CARTESIAN_POINT('Ctrl Pts',(7.17257573845094,-1.30008806150181,6.89309825403218));
#17846=CARTESIAN_POINT('Ctrl Pts',(7.12769372870001,-1.36687124932412,6.8889111074519));
#17847=CARTESIAN_POINT('Ctrl Pts',(7.08273896064388,-1.43376269949007,6.8847171730809));
#17848=CARTESIAN_POINT('Ctrl Pts',(7.03454762087581,-1.49833438387594,6.88052323870991));
#17849=CARTESIAN_POINT('Ctrl Pts',(6.98340547657638,-1.56027049524785,6.87632930433892));
#17850=CARTESIAN_POINT('Ctrl Pts',(6.96705959253493,-1.580066311562,6.87498885282198));
#17851=CARTESIAN_POINT('Ctrl Pts',(6.95041254789922,-1.59959317725488,6.87364840130504));
#17852=CARTESIAN_POINT('Ctrl Pts',(6.93347442743153,-1.61884161198753,6.8723079497881));
#17853=CARTESIAN_POINT('Ctrl Pts',(6.87999718967411,-1.67961300174232,6.86807586012913));
#17854=CARTESIAN_POINT('Ctrl Pts',(6.82340565434217,-1.73784503569689,6.86384377047017));
#17855=CARTESIAN_POINT('Ctrl Pts',(6.7639703595767,-1.79320158591269,6.8596116808112));
#17856=CARTESIAN_POINT('Ctrl Pts',(6.70462001204295,-1.8484790183969,6.85538563981915));
#17857=CARTESIAN_POINT('Ctrl Pts',(6.64243431464168,-1.90088881549508,6.8511595988271));
#17858=CARTESIAN_POINT('Ctrl Pts',(6.57772292224269,-1.95012912477712,6.84693355783504));
#17859=CARTESIAN_POINT('Ctrl Pts',(6.51299373046219,-1.9993829779966,6.84270635443691));
#17860=CARTESIAN_POINT('Ctrl Pts',(6.4457377819112,-2.04546526724344,6.83847915103878));
#17861=CARTESIAN_POINT('Ctrl Pts',(6.37630071801608,-2.08811202078027,6.83425194764065));
#17862=CARTESIAN_POINT('Ctrl Pts',(6.30700696413248,-2.13067075638548,6.83003346869793));
#17863=CARTESIAN_POINT('Ctrl Pts',(6.23554147196011,-2.16980785869417,6.82581498975521));
#17864=CARTESIAN_POINT('Ctrl Pts',(6.16227797187641,-2.20530340381644,6.82159651081248));
#17865=CARTESIAN_POINT('Ctrl Pts',(6.08903849658266,-2.24078730913151,6.81737941520622));
#17866=CARTESIAN_POINT('Ctrl Pts',(6.01400260215468,-2.2726318262804,6.81316231959995));
#17867=CARTESIAN_POINT('Ctrl Pts',(5.93756795157072,-2.30066332151552,6.80894522399368));
#17868=CARTESIAN_POINT('Ctrl Pts',(5.86113497830319,-2.32869420161487,6.80472822092926));
#17869=CARTESIAN_POINT('Ctrl Pts',(5.78330374658018,-2.35291206724811,6.80051121786484));
#17870=CARTESIAN_POINT('Ctrl Pts',(5.70448984443593,-2.37319222362713,6.79629421480041));
#17871=CARTESIAN_POINT('Ctrl Pts',(5.62534965112445,-2.39355634026844,6.79205975325704));
#17872=CARTESIAN_POINT('Ctrl Pts',(5.5452190872179,-2.40994994376381,6.78782529171366));
#17873=CARTESIAN_POINT('Ctrl Pts',(5.46453034046881,-2.42229837109701,6.78359083017028));
#17874=CARTESIAN_POINT('Ctrl Pts',(5.38405776682911,-2.43461371577568,6.77936771316695));
#17875=CARTESIAN_POINT('Ctrl Pts',(5.30303046671893,-2.44290552482377,6.77514459616361));
#17876=CARTESIAN_POINT('Ctrl Pts',(5.22188154726461,-2.44715187978552,6.77092147916028));
#17877=CARTESIAN_POINT('Ctrl Pts',(5.14040564284918,-2.45141534519336,6.76668134534688));
#17878=CARTESIAN_POINT('Ctrl Pts',(5.05880760837002,-2.45160069338739,6.76244121153348));
#17879=CARTESIAN_POINT('Ctrl Pts',(4.97752315877344,-2.4477384726225,6.75820107772008));
#17880=CARTESIAN_POINT('Ctrl Pts',(4.89623870917688,-2.44387625185761,6.75396094390668));
#17881=CARTESIAN_POINT('Ctrl Pts',(4.8152683035326,-2.43596656948219,6.74972081009328));
#17882=CARTESIAN_POINT('Ctrl Pts',(4.73503801466492,-2.4240917066919,6.74548067627989));
#17883=CARTESIAN_POINT('Ctrl Pts',(4.65495993439775,-2.41223937225435,6.74124858662092));
#17884=CARTESIAN_POINT('Ctrl Pts',(4.57532040791192,-2.39639268582382,6.73701649696195));
#17885=CARTESIAN_POINT('Ctrl Pts',(4.49654862582741,-2.37659601279817,6.73278440730299));
#17886=CARTESIAN_POINT('Ctrl Pts',(4.41788942743332,-2.3568276339465,6.72855836631093));
#17887=CARTESIAN_POINT('Ctrl Pts',(4.34009595714923,-2.33312059334013,6.72433232531888));
#17888=CARTESIAN_POINT('Ctrl Pts',(4.26358989930911,-2.30557072077837,6.72010628432683));
#17889=CARTESIAN_POINT('Ctrl Pts',(4.18706279787122,-2.27801327040573,6.71587908092869));
#17890=CARTESIAN_POINT('Ctrl Pts',(4.11182427435442,-2.24661096831282,6.71165187753056));
#17891=CARTESIAN_POINT('Ctrl Pts',(4.03828377926908,-2.21151044107732,6.70742467413243));
#17892=CARTESIAN_POINT('Ctrl Pts',(3.96489506319927,-2.17648235724137,6.70320619518971));
#17893=CARTESIAN_POINT('Ctrl Pts',(3.89319780366043,-2.13777147604273,6.69898771624699));
#17894=CARTESIAN_POINT('Ctrl Pts',(3.82357974790947,-2.09557194427408,6.69476923730427));
#17895=CARTESIAN_POINT('Ctrl Pts',(3.75398452152329,-2.05338625070436,6.690552141698));
#17896=CARTESIAN_POINT('Ctrl Pts',(3.68646754197144,-2.00771441915321,6.68633504609174));
#17897=CARTESIAN_POINT('Ctrl Pts',(3.62139071185994,-1.95879584683516,6.68211795048548));
#17898=CARTESIAN_POINT('Ctrl Pts',(3.5563153098237,-1.9098783480083,6.67790094742106));
#17899=CARTESIAN_POINT('Ctrl Pts',(3.49368032151697,-1.85771453021127,6.67368394435664));
#17900=CARTESIAN_POINT('Ctrl Pts',(3.43381631600644,-1.8025854384521,6.66946694129222));
#17901=CARTESIAN_POINT('Ctrl Pts',(3.37370447228837,-1.74722811112519,6.66523247974884));
#17902=CARTESIAN_POINT('Ctrl Pts',(3.31638695987383,-1.68888121507957,6.66099801820546));
#17903=CARTESIAN_POINT('Ctrl Pts',(3.26216137660258,-1.62786692471709,6.65676355666208));
#17904=CARTESIAN_POINT('Ctrl Pts',(3.20808106901624,-1.56701609765528,6.65254043965875));
#17905=CARTESIAN_POINT('Ctrl Pts',(3.1570764052606,-1.50351254078169,6.64831732265541));
#17906=CARTESIAN_POINT('Ctrl Pts',(3.10940121141798,-1.43770787110605,6.64409420565208));
#17907=CARTESIAN_POINT('Ctrl Pts',(3.06153391308996,-1.37163804525199,6.63985407183868));
#17908=CARTESIAN_POINT('Ctrl Pts',(3.01702322307941,-1.30324892287414,6.63561393802528));
#17909=CARTESIAN_POINT('Ctrl Pts',(2.97608034673313,-1.23292282976524,6.63137380421188));
#17910=CARTESIAN_POINT('Ctrl Pts',(2.93513747038684,-1.16259673665634,6.62713367039847));
#17911=CARTESIAN_POINT('Ctrl Pts',(2.89776256714265,-1.09033411649224,6.62289353658507));
#17912=CARTESIAN_POINT('Ctrl Pts',(2.86411817867461,-1.01653732291213,6.61865340277167));
#17913=CARTESIAN_POINT('Ctrl Pts',(2.83053761853579,-0.942880532650582,
6.61442131311271));
#17914=CARTESIAN_POINT('Ctrl Pts',(2.80054813471462,-0.867420592882331,
6.61018922345375));
#17915=CARTESIAN_POINT('Ctrl Pts',(2.77434578854561,-0.790541863893945,
6.60595713379479));
#17916=CARTESIAN_POINT('Ctrl Pts',(2.74818089178745,-0.713773012971022,
6.60173109280275));
#17917=CARTESIAN_POINT('Ctrl Pts',(2.72579253108134,-0.63558983640461,6.59750505181071));
#17918=CARTESIAN_POINT('Ctrl Pts',(2.7073294904886,-0.556398369083661,6.59327901081866));
#17919=CARTESIAN_POINT('Ctrl Pts',(2.68886137149012,-0.477185119521554,
6.58905180742053));
#17920=CARTESIAN_POINT('Ctrl Pts',(2.67432090143951,-0.396963459550963,
6.5848246040224));
#17921=CARTESIAN_POINT('Ctrl Pts',(2.66380757770076,-0.316156767664846,
6.58059740062426));
#17922=CARTESIAN_POINT('Ctrl Pts',(2.65331595223757,-0.235516851378036,
6.57637892168154));
#17923=CARTESIAN_POINT('Ctrl Pts',(2.6468349513143,-0.154294773248997,6.57216044273881));
#17924=CARTESIAN_POINT('Ctrl Pts',(2.64441238840444,-0.0729215260666718,
6.56794196379609));
#17925=CARTESIAN_POINT('Ctrl Pts',(2.64199061990878,0.00842503695261541,
6.56372486818982));
#17926=CARTESIAN_POINT('Ctrl Pts',(2.64362466028642,0.0899222064561095,
6.55950777258356));
#17927=CARTESIAN_POINT('Ctrl Pts',(2.64931029310316,0.1711360852852,6.55529067697729));
#17928=CARTESIAN_POINT('Ctrl Pts',(2.6549958011518,0.252348181920348,6.55107367391288));
#17929=CARTESIAN_POINT('Ctrl Pts',(2.66473269126401,0.333276536767597,6.54685667084846));
#17930=CARTESIAN_POINT('Ctrl Pts',(2.67846475733505,0.413490913754334,6.54263966778404));
#17931=CARTESIAN_POINT('Ctrl Pts',(2.69225367444059,0.494037379902969,6.53840520624066));
#17932=CARTESIAN_POINT('Ctrl Pts',(2.71007085127474,0.573863476620917,6.53417074469728));
#17933=CARTESIAN_POINT('Ctrl Pts',(2.73180763696923,0.652544285318017,6.5299362831539));
#17934=CARTESIAN_POINT('Ctrl Pts',(2.7534861876713,0.731014300369605,6.52571316615056));
#17935=CARTESIAN_POINT('Ctrl Pts',(2.77906318609842,0.80834472524806,6.52149004914723));
#17936=CARTESIAN_POINT('Ctrl Pts',(2.80838147504338,0.88413137705688,6.5172669321439));
#17937=CARTESIAN_POINT('Ctrl Pts',(2.83781790036826,0.960223406874211,6.51302679833049));
#17938=CARTESIAN_POINT('Ctrl Pts',(2.87102563075637,1.03475876913479,6.50878666451708));
#17939=CARTESIAN_POINT('Ctrl Pts',(2.90779856556206,1.10735236224923,6.50454653070368));
#17940=CARTESIAN_POINT('Ctrl Pts',(2.94457150036774,1.17994595536366,6.50030639689027));
#17941=CARTESIAN_POINT('Ctrl Pts',(2.98490935385593,1.25059740433307,6.49606626307686));
#17942=CARTESIAN_POINT('Ctrl Pts',(3.02856276223631,1.31895156700724,6.49182612926345));
#17943=CARTESIAN_POINT('Ctrl Pts',(3.07213335371169,1.38717605183019,6.48759403960449));
#17944=CARTESIAN_POINT('Ctrl Pts',(3.11916947096469,1.45336649920331,6.48336194994553));
#17945=CARTESIAN_POINT('Ctrl Pts',(3.16945507369038,1.51714941285694,6.47912986028657));
#17946=CARTESIAN_POINT('Ctrl Pts',(3.21966880627954,1.58084116549303,6.47490381929453));
#17947=CARTESIAN_POINT('Ctrl Pts',(3.27312251498226,1.64213185662184,6.47067777830248));
#17948=CARTESIAN_POINT('Ctrl Pts',(3.32955626775308,1.70067589058414,6.46645173731044));
#17949=CARTESIAN_POINT('Ctrl Pts',(3.38600554307516,1.75923602754727,6.46222453391231));
#17950=CARTESIAN_POINT('Ctrl Pts',(3.44543622880718,1.81504761766214,6.45799733051417));
#17951=CARTESIAN_POINT('Ctrl Pts',(3.50754704413236,1.86779700675106,6.45377012711604));
#17952=CARTESIAN_POINT('Ctrl Pts',(3.56952966996961,1.92043752724536,6.44955164817332));
#17953=CARTESIAN_POINT('Ctrl Pts',(3.6341810354678,1.97002815426071,6.4453331692306));
#17954=CARTESIAN_POINT('Ctrl Pts',(3.70116537433277,2.01629447586574,6.44111469028788));
#17955=CARTESIAN_POINT('Ctrl Pts',(3.76812774748944,2.06254562567776,6.43689759468161));
#17956=CARTESIAN_POINT('Ctrl Pts',(3.83742119266684,2.10547437106466,6.43268049907535));
#17957=CARTESIAN_POINT('Ctrl Pts',(3.90867922331442,2.1448483929983,6.42846340346908));
#17958=CARTESIAN_POINT('Ctrl Pts',(3.97993569024362,2.18422155089064,6.42424640040467));
#17959=CARTESIAN_POINT('Ctrl Pts',(4.05315624964168,2.22003991669329,6.42002939734025));
#17960=CARTESIAN_POINT('Ctrl Pts',(4.12794922733439,2.25211679936301,6.41581239427583));
#17961=CARTESIAN_POINT('Ctrl Pts',(4.203051849485,2.28432648098327,6.41157793273245));
#17962=CARTESIAN_POINT('Ctrl Pts',(4.27973950882041,2.31276343604563,6.40734347118907));
#17963=CARTESIAN_POINT('Ctrl Pts',(4.35759648647074,2.33728788386236,6.40310900964568));
#17964=CARTESIAN_POINT('Ctrl Pts',(4.43524487760014,2.36174662826492,6.39888589264235));
#17965=CARTESIAN_POINT('Ctrl Pts',(4.51405586678756,2.38231372440704,6.39466277563902));
#17966=CARTESIAN_POINT('Ctrl Pts',(4.5936047727012,2.3989013772546,6.39043965863569));
#17967=CARTESIAN_POINT('Ctrl Pts',(4.67347421641258,2.41555586910707,6.38619952482228));
#17968=CARTESIAN_POINT('Ctrl Pts',(4.75408706910091,2.42819871555458,6.38195939100887));
#17969=CARTESIAN_POINT('Ctrl Pts',(4.83500806075281,2.43679357480656,6.37771925719546));
#17970=CARTESIAN_POINT('Ctrl Pts',(4.91592905240472,2.44538843405854,6.37347912338205));
#17971=CARTESIAN_POINT('Ctrl Pts',(4.99715771294223,2.44993534210655,6.36923898956864));
#17972=CARTESIAN_POINT('Ctrl Pts',(5.07826040200378,2.45045055575236,6.36499885575523));
#17973=CARTESIAN_POINT('Ctrl Pts',(5.15920922739352,2.45096479196247,6.36076676609628));
#17974=CARTESIAN_POINT('Ctrl Pts',(5.24033456232364,2.44746455166315,6.35653467643732));
#17975=CARTESIAN_POINT('Ctrl Pts',(5.32120547477914,2.43992814441337,6.35230258677837));
#17976=CARTESIAN_POINT('Ctrl Pts',(5.40196080338581,2.43240250848952,6.34807654578631));
#17977=CARTESIAN_POINT('Ctrl Pts',(5.4824619729098,2.42085220553111,6.34385050479426));
#17978=CARTESIAN_POINT('Ctrl Pts',(5.56227761120317,2.40530755216616,6.3396244638022));
#17979=CARTESIAN_POINT('Ctrl Pts',(5.64211520342061,2.38975862312107,6.33539726040407));
#17980=CARTESIAN_POINT('Ctrl Pts',(5.72126642100705,2.37021316962647,6.33117005700593));
#17981=CARTESIAN_POINT('Ctrl Pts',(5.79930422572376,2.34675357746022,6.3269428536078));
#17982=CARTESIAN_POINT('Ctrl Pts',(5.87718096950162,2.32334240315956,6.32272437466508));
#17983=CARTESIAN_POINT('Ctrl Pts',(5.95394843948702,2.29603334055059,6.31850589572237));
#17984=CARTESIAN_POINT('Ctrl Pts',(6.0291937900519,2.26495905236261,6.31428741677965));
#17985=CARTESIAN_POINT('Ctrl Pts',(6.10441446593234,2.23389495414982,6.31007032117339));
#17986=CARTESIAN_POINT('Ctrl Pts',(6.1781135844623,2.19906825960485,6.30585322556713));
#17987=CARTESIAN_POINT('Ctrl Pts',(6.24989693204442,2.16066029760629,6.30163612996087));
#17988=CARTESIAN_POINT('Ctrl Pts',(6.32167870438045,2.12225317844935,6.29741912689646));
#17989=CARTESIAN_POINT('Ctrl Pts',(6.39154438017218,2.08026516833344,6.29320212383205));
#17990=CARTESIAN_POINT('Ctrl Pts',(6.45912435248052,2.03492354003513,6.28898512076764));
#17991=CARTESIAN_POINT('Ctrl Pts',(6.52698410725699,1.98939419646791,6.28475065922425));
#17992=CARTESIAN_POINT('Ctrl Pts',(6.59253879355058,1.94048365964281,6.28051619768086));
#17993=CARTESIAN_POINT('Ctrl Pts',(6.65544510872075,1.88846488398174,6.27628173613747));
#17994=CARTESIAN_POINT('Ctrl Pts',(6.71818289166911,1.83658547175047,6.27205861913414));
#17995=CARTESIAN_POINT('Ctrl Pts',(6.77828615862546,1.78161479991907,6.26783550213081));
#17996=CARTESIAN_POINT('Ctrl Pts',(6.83545036964551,1.72386160401179,6.26361238512748));
#17997=CARTESIAN_POINT('Ctrl Pts',(6.8928449206068,1.66587569488215,6.25937225131407));
#17998=CARTESIAN_POINT('Ctrl Pts',(6.9472763720494,1.60508514727229,6.25513211750066));
#17999=CARTESIAN_POINT('Ctrl Pts',(6.99847761586162,1.54183555337969,6.25089198368725));
#18000=CARTESIAN_POINT('Ctrl Pts',(7.04967885967384,1.47858595948709,6.24665184987383));
#18001=CARTESIAN_POINT('Ctrl Pts',(7.09764967054014,1.41287773343925,6.24241171606042));
#18002=CARTESIAN_POINT('Ctrl Pts',(7.14216797518798,1.34508369115378,6.23817158224701));
#18003=CARTESIAN_POINT('Ctrl Pts',(7.18746672627465,1.27610115754336,6.23385711502488));
#18004=CARTESIAN_POINT('Ctrl Pts',(7.22935510164734,1.20470926392168,6.22954264780275));
#18005=CARTESIAN_POINT('Ctrl Pts',(7.26757389031831,1.13127157776675,6.22522818058062));
#18006=CARTESIAN_POINT('Ctrl Pts',(7.30573175456386,1.05795095834756,6.22092059103425));
#18007=CARTESIAN_POINT('Ctrl Pts',(7.34023145647764,0.982591415569505,6.21661300148789));
#18008=CARTESIAN_POINT('Ctrl Pts',(7.37085724304496,0.905585020967907,6.21230541194152));
#18009=CARTESIAN_POINT('Ctrl Pts',(7.40143315944292,0.828704021413127,6.2080048367528));
#18010=CARTESIAN_POINT('Ctrl Pts',(7.42814755207734,0.750181913787023,6.20370426156408));
#18011=CARTESIAN_POINT('Ctrl Pts',(7.45083143436958,0.670433500930149,6.19940368637536));
#18012=CARTESIAN_POINT('Ctrl Pts',(7.47349353380069,0.590761668818158,6.19510724093969));
#18013=CARTESIAN_POINT('Ctrl Pts',(7.49213269474097,0.509866293854989,6.19081079550403));
#18014=CARTESIAN_POINT('Ctrl Pts',(7.50662893554642,0.42817965852963,6.18651435006836));
#18015=CARTESIAN_POINT('Ctrl Pts',(7.52111435624942,0.346553994719236,6.18222111153167));
#18016=CARTESIAN_POINT('Ctrl Pts',(7.53146292938353,0.264138678008879,6.17792787299498));
#18017=CARTESIAN_POINT('Ctrl Pts',(7.53760547669647,0.181377414859107,6.17363463445829));
#18018=CARTESIAN_POINT('Ctrl Pts',(7.54210976449276,0.120689148474039,6.17048643209823));
#18019=CARTESIAN_POINT('Ctrl Pts',(7.54435344337769,0.0598151464488679,
6.16733822973817));
#18020=CARTESIAN_POINT('Ctrl Pts',(7.54432692296591,-0.0010674360424196,
6.16419002737812));
#18021=CARTESIAN_POINT('',(7.54432671099194,-0.00147590784951504,5.36419002740651));
#18022=CARTESIAN_POINT('Ctrl Pts',(7.54432692296551,-0.00106743696241388,
6.16419002733055));
#18023=CARTESIAN_POINT('Ctrl Pts',(7.54428806046215,-0.0902835300895011,
6.15957671588008));
#18024=CARTESIAN_POINT('Ctrl Pts',(7.53937283421591,-0.179342371974235,
6.15496340442961));
#18025=CARTESIAN_POINT('Ctrl Pts',(7.529657579374,-0.267731947853424,6.15035009297914));
#18026=CARTESIAN_POINT('Ctrl Pts',(7.51991365953643,-0.356382318415845,
6.14572316988854));
#18027=CARTESIAN_POINT('Ctrl Pts',(7.50534147059154,-0.444359170624297,
6.14109624679794));
#18028=CARTESIAN_POINT('Ctrl Pts',(7.48606828497605,-0.531161583907186,
6.13646932370734));
#18029=CARTESIAN_POINT('Ctrl Pts',(7.46670910596212,-0.618351293543685,
6.13182175613954));
#18030=CARTESIAN_POINT('Ctrl Pts',(7.44260702225196,-0.70435577060529,6.12717418857175));
#18031=CARTESIAN_POINT('Ctrl Pts',(7.41393969617488,-0.78868754800971,6.12252662100395));
#18032=CARTESIAN_POINT('Ctrl Pts',(7.39094795642252,-0.856323234495553,
6.11879918358224));
#18033=CARTESIAN_POINT('Ctrl Pts',(7.36502066814126,-0.922883320604722,
6.11507174616052));
#18034=CARTESIAN_POINT('Ctrl Pts',(7.33627098328143,-0.988127486225679,
6.1113443087388));
#18035=CARTESIAN_POINT('Ctrl Pts',(7.30362892112772,-1.06220496289194,6.10711221907984));
#18036=CARTESIAN_POINT('Ctrl Pts',(7.26725138371582,-1.13480142576412,6.10288012942087));
#18037=CARTESIAN_POINT('Ctrl Pts',(7.22729484661249,-1.20551477003771,6.09864803976191));
#18038=CARTESIAN_POINT('Ctrl Pts',(7.18739541694389,-1.27612704805317,6.09442199876986));
#18039=CARTESIAN_POINT('Ctrl Pts',(7.14392737370826,-1.34486115174563,6.09019595777781));
#18040=CARTESIAN_POINT('Ctrl Pts',(7.09709482980952,-1.41133584765593,6.08596991678576));
#18041=CARTESIAN_POINT('Ctrl Pts',(7.05024940424823,-1.47782882795843,6.08174271338763));
#18042=CARTESIAN_POINT('Ctrl Pts',(7.0000378391584,-1.54206074159141,6.0775155099895));
#18043=CARTESIAN_POINT('Ctrl Pts',(6.94670998865645,-1.60367560822642,6.07328830659137));
#18044=CARTESIAN_POINT('Ctrl Pts',(6.89349220062604,-1.66516330895391,6.06906982764864));
#18045=CARTESIAN_POINT('Ctrl Pts',(6.83717126285874,-1.7240443867088,6.06485134870591));
#18046=CARTESIAN_POINT('Ctrl Pts',(6.77803710266931,-1.77999637743957,6.06063286976319));
#18047=CARTESIAN_POINT('Ctrl Pts',(6.71892233393374,-1.83593002022319,6.05641577415692));
#18048=CARTESIAN_POINT('Ctrl Pts',(6.65699651209779,-1.88893616434808,6.05219867855066));
#18049=CARTESIAN_POINT('Ctrl Pts',(6.59258635189059,-1.93872925420082,6.0479815829444));
#18050=CARTESIAN_POINT('Ctrl Pts',(6.52817760512899,-1.98852125137154,6.04376457987998));
#18051=CARTESIAN_POINT('Ctrl Pts',(6.46128499673565,-2.03510005115936,6.03954757681556));
#18052=CARTESIAN_POINT('Ctrl Pts',(6.39226710089295,-2.07822134482499,6.03533057375114));
#18053=CARTESIAN_POINT('Ctrl Pts',(6.32296346954942,-2.12152116152861,6.03109611220776));
#18054=CARTESIAN_POINT('Ctrl Pts',(6.25151730910728,-2.16133452191967,6.02686165066438));
#18055=CARTESIAN_POINT('Ctrl Pts',(6.17831811948958,-2.19745980598582,6.022627189121));
#18056=CARTESIAN_POINT('Ctrl Pts',(6.10531503771918,-2.23348830685357,6.01840407211766));
#18057=CARTESIAN_POINT('Ctrl Pts',(6.0305687533014,-2.26584831961888,6.01418095511433));
#18058=CARTESIAN_POINT('Ctrl Pts',(5.95448556150817,-2.29438823177046,6.00995783811099));
#18059=CARTESIAN_POINT('Ctrl Pts',(5.87809579681561,-2.32304314387681,6.00571770429759));
#18060=CARTESIAN_POINT('Ctrl Pts',(5.80035877977824,-2.34784696952846,6.00147757048419));
#18061=CARTESIAN_POINT('Ctrl Pts',(5.72169912686958,-2.36869732923174,5.99723743667079));
#18062=CARTESIAN_POINT('Ctrl Pts',(5.64303947396092,-2.38954768893503,5.99299730285739));
#18063=CARTESIAN_POINT('Ctrl Pts',(5.5634576552422,-2.40644454648054,5.98875716904398));
#18064=CARTESIAN_POINT('Ctrl Pts',(5.48338470822629,-2.41933775299716,5.98451703523058));
#18065=CARTESIAN_POINT('Ctrl Pts',(5.40346367131052,-2.43220649921395,5.98028494557161));
#18066=CARTESIAN_POINT('Ctrl Pts',(5.32275520129984,-2.44113479794551,5.97605285591265));
#18067=CARTESIAN_POINT('Ctrl Pts',(5.2416818647386,-2.44603541162881,5.97182076625369));
#18068=CARTESIAN_POINT('Ctrl Pts',(5.16072440133893,-2.45092902116469,5.96759472526164));
#18069=CARTESIAN_POINT('Ctrl Pts',(5.07940356707358,-2.4518063509304,5.9633686842696));
#18070=CARTESIAN_POINT('Ctrl Pts',(4.99815030471609,-2.44863149335155,5.95914264327755));
#18071=CARTESIAN_POINT('Ctrl Pts',(4.91687469300443,-2.44545576250295,5.95491543987942));
#18072=CARTESIAN_POINT('Ctrl Pts',(4.83566715474355,-2.4382255669776,5.95068823648129));
#18073=CARTESIAN_POINT('Ctrl Pts',(4.75496230035753,-2.4269571195184,5.94646103308316));
#18074=CARTESIAN_POINT('Ctrl Pts',(4.67442401139009,-2.41571192882215,5.94224255414043));
#18075=CARTESIAN_POINT('Ctrl Pts',(4.59438679711931,-2.40044517801083,5.93802407519771));
#18076=CARTESIAN_POINT('Ctrl Pts',(4.51527891886783,-2.38122493434452,5.93380559625499));
#18077=CARTESIAN_POINT('Ctrl Pts',(4.43619698191265,-2.36201099343903,5.92958850064872));
#18078=CARTESIAN_POINT('Ctrl Pts',(4.35804422697275,-2.33884624391854,5.92537140504246));
#18079=CARTESIAN_POINT('Ctrl Pts',(4.28123793294667,-2.31184969352819,5.92115430943619));
#18080=CARTESIAN_POINT('Ctrl Pts',(4.20443332439258,-2.28485373556233,5.91693730637178));
#18081=CARTESIAN_POINT('Ctrl Pts',(4.1289755560197,-2.25402629908897,5.91272030330736));
#18082=CARTESIAN_POINT('Ctrl Pts',(4.0552646040617,-2.21953555431026,5.90850330024295));
#18083=CARTESIAN_POINT('Ctrl Pts',(3.98124848725447,-2.18490201714249,5.90426883869957));
#18084=CARTESIAN_POINT('Ctrl Pts',(3.90899411417667,-2.14657496300716,5.90003437715618));
#18085=CARTESIAN_POINT('Ctrl Pts',(3.83888244061978,-2.10477172460861,5.8957999156128));
#18086=CARTESIAN_POINT('Ctrl Pts',(3.76895860315025,-2.06308048120806,5.89157679860947));
#18087=CARTESIAN_POINT('Ctrl Pts',(3.70116636520282,-2.0179319492883,5.88735368160613));
#18088=CARTESIAN_POINT('Ctrl Pts',(3.63585383805489,-1.96958474195827,5.8831305646028));
#18089=CARTESIAN_POINT('Ctrl Pts',(3.57027813778892,-1.92104272230268,5.87889043078939));
#18090=CARTESIAN_POINT('Ctrl Pts',(3.5072025331765,-1.86927650081016,5.87465029697599));
#18091=CARTESIAN_POINT('Ctrl Pts',(3.44694377047311,-1.81458683073498,5.87041016316258));
#18092=CARTESIAN_POINT('Ctrl Pts',(3.38668500776971,-1.75989716065979,5.86617002934918));
#18093=CARTESIAN_POINT('Ctrl Pts',(3.32924337288418,-1.70228441686835,5.86192989553577));
#18094=CARTESIAN_POINT('Ctrl Pts',(3.27489526229108,-1.64208313371705,5.85768976172237));
#18095=CARTESIAN_POINT('Ctrl Pts',(3.22065025801835,-1.58199606121114,5.8534576720634));
#18096=CARTESIAN_POINT('Ctrl Pts',(3.16928466213752,-1.5191061000925,5.84922558240444));
#18097=CARTESIAN_POINT('Ctrl Pts',(3.12110139711799,-1.45372051385441,5.84499349274548));
#18098=CARTESIAN_POINT('Ctrl Pts',(3.07298699749229,-1.38842837923577,5.84076745175344));
#18099=CARTESIAN_POINT('Ctrl Pts',(3.02804616865437,-1.3206480746002,5.83654141076139));
#18100=CARTESIAN_POINT('Ctrl Pts',(2.98654330204953,-1.25072179607799,5.83231536976935));
#18101=CARTESIAN_POINT('Ctrl Pts',(2.94502901975211,-1.18077628377836,5.82808816637121));
#18102=CARTESIAN_POINT('Ctrl Pts',(2.90695488381134,-1.10868398065182,5.82386096297308));
#18103=CARTESIAN_POINT('Ctrl Pts',(2.8725435317881,-1.03481849289507,5.81963375957495));
#18104=CARTESIAN_POINT('Ctrl Pts',(2.83820320078704,-0.961105454900868,
5.81541528063222));
#18105=CARTESIAN_POINT('Ctrl Pts',(2.80751076859188,-0.885626954952176,
5.8111968016895));
#18106=CARTESIAN_POINT('Ctrl Pts',(2.78064189706718,-0.808779457198316,
5.80697832274678));
#18107=CARTESIAN_POINT('Ctrl Pts',(2.75378183646463,-0.731957159509913,
5.80276122714051));
#18108=CARTESIAN_POINT('Ctrl Pts',(2.73074299978356,-0.653767193853057,
5.79854413153425));
#18109=CARTESIAN_POINT('Ctrl Pts',(2.71165232180659,-0.574624496468061,
5.79432703592799));
#18110=CARTESIAN_POINT('Ctrl Pts',(2.69256206276406,-0.49548353582608,5.79011003286357));
#18111=CARTESIAN_POINT('Ctrl Pts',(2.67741989801101,-0.415390337026624,
5.78589302979915));
#18112=CARTESIAN_POINT('Ctrl Pts',(2.66630209208741,-0.334772036961481,
5.78167602673474));
#18113=CARTESIAN_POINT('Ctrl Pts',(2.65513825821981,-0.253819975484631,
5.77744156519135));
#18114=CARTESIAN_POINT('Ctrl Pts',(2.64803225323112,-0.172338921240949,
5.77320710364797));
#18115=CARTESIAN_POINT('Ctrl Pts',(2.6450087376301,-0.0907667699700236,
5.76897264210459));
#18116=CARTESIAN_POINT('Ctrl Pts',(2.64199332232552,-0.00941315853644546,
5.76474952510125));
#18117=CARTESIAN_POINT('Ctrl Pts',(2.64303850239018,0.0720305954233322,
5.76052640809792));
#18118=CARTESIAN_POINT('Ctrl Pts',(2.64811643569602,0.153131725208303,5.75630329109459));
#18119=CARTESIAN_POINT('Ctrl Pts',(2.65321483024567,0.23455964738884,5.75206315728118));
#18120=CARTESIAN_POINT('Ctrl Pts',(2.66237848463236,0.31564171089935,5.74782302346777));
#18121=CARTESIAN_POINT('Ctrl Pts',(2.67552713668527,0.395948568917041,5.74358288965437));
#18122=CARTESIAN_POINT('Ctrl Pts',(2.68867578873818,0.476255426934721,5.73934275584096));
#18123=CARTESIAN_POINT('Ctrl Pts',(2.70580927922513,0.555786635709889,5.73510262202755));
#18124=CARTESIAN_POINT('Ctrl Pts',(2.72679705821167,0.634128353531991,5.73086248821415));
#18125=CARTESIAN_POINT('Ctrl Pts',(2.74774502030964,0.712321445649041,5.72663039855518));
#18126=CARTESIAN_POINT('Ctrl Pts',(2.77261079716259,0.789621282590665,5.72239830889622));
#18127=CARTESIAN_POINT('Ctrl Pts',(2.80130114784229,0.865606581784123,5.71816621923726));
#18128=CARTESIAN_POINT('Ctrl Pts',(2.82995049315846,0.941483279836682,5.71394017824521));
#18129=CARTESIAN_POINT('Ctrl Pts',(2.86241339300269,1.01604874051948,5.70971413725316));
#18130=CARTESIAN_POINT('Ctrl Pts',(2.89854634077541,1.08889503383384,5.70548809626112));
#18131=CARTESIAN_POINT('Ctrl Pts',(2.93468922720194,1.16176136409883,5.70126089286298));
#18132=CARTESIAN_POINT('Ctrl Pts',(2.97450403450886,1.23290713780914,5.69703368946485));
#18133=CARTESIAN_POINT('Ctrl Pts',(3.01779819523461,1.3019423974716,5.69280648606672));
#18134=CARTESIAN_POINT('Ctrl Pts',(3.06100300185573,1.37083517639966,5.688588007124));
#18135=CARTESIAN_POINT('Ctrl Pts',(3.10767258855504,1.4376257373037,5.68436952818128));
#18136=CARTESIAN_POINT('Ctrl Pts',(3.15756966680863,1.50195112692396,5.68015104923855));
#18137=CARTESIAN_POINT('Ctrl Pts',(3.20745038266037,1.56625542276659,5.67593395363229));
#18138=CARTESIAN_POINT('Ctrl Pts',(3.26055620364708,1.62809578581827,5.67171685802603));
#18139=CARTESIAN_POINT('Ctrl Pts',(3.31660784946632,1.68714012116002,5.66749976241976));
#18140=CARTESIAN_POINT('Ctrl Pts',(3.37265826526298,1.74618316080626,5.66328275935535));
#18141=CARTESIAN_POINT('Ctrl Pts',(3.43165405659566,1.80242995851394,5.65906575629093));
#18142=CARTESIAN_POINT('Ctrl Pts',(3.49327815909478,1.8555843177437,5.65484875322651));
#18143=CARTESIAN_POINT('Ctrl Pts',(3.55515738663906,1.90895873710819,5.65061429168313));
#18144=CARTESIAN_POINT('Ctrl Pts',(3.61968638538108,1.95921474002239,5.64637983013975));
#18145=CARTESIAN_POINT('Ctrl Pts',(3.68651100948259,2.00609359584509,5.64214536859637));
#18146=CARTESIAN_POINT('Ctrl Pts',(3.75315660382636,2.05284685859018,5.63792225159303));
#18147=CARTESIAN_POINT('Ctrl Pts',(3.82208512119672,2.0962408322911,5.6336991345897));
#18148=CARTESIAN_POINT('Ctrl Pts',(3.8929181814293,2.136063642804,5.62947601758637));
#18149=CARTESIAN_POINT('Ctrl Pts',(3.96403665945442,2.17604691706972,5.62523588377296));
#18150=CARTESIAN_POINT('Ctrl Pts',(4.03707463540399,2.21242998530243,5.62099574995956));
#18151=CARTESIAN_POINT('Ctrl Pts',(4.11162810508852,2.24504683146319,5.61675561614615));
#18152=CARTESIAN_POINT('Ctrl Pts',(4.18618157477304,2.27766367762394,5.61251548233275));
#18153=CARTESIAN_POINT('Ctrl Pts',(4.26225007917262,2.30651419415162,5.60827534851934));
#18154=CARTESIAN_POINT('Ctrl Pts',(4.33941529296307,2.33148300266897,5.60403521470594));
#18155=CARTESIAN_POINT('Ctrl Pts',(4.41643411304883,2.35640444170205,5.59980312504697));
#18156=CARTESIAN_POINT('Ctrl Pts',(4.49483282171879,2.37755187957483,5.59557103538801));
#18157=CARTESIAN_POINT('Ctrl Pts',(4.57420712856542,2.39477457762881,5.59133894572905));
#18158=CARTESIAN_POINT('Ctrl Pts',(4.65346799056978,2.41197266033379,5.587112904737));
#18159=CARTESIAN_POINT('Ctrl Pts',(4.73370123106812,2.42525704636648,5.58288686374496));
#18160=CARTESIAN_POINT('Ctrl Pts',(4.8144864437794,2.43452644610849,5.57866082275291));
#18161=CARTESIAN_POINT('Ctrl Pts',(4.89529387710407,2.44379839547241,5.57443361935478));
#18162=CARTESIAN_POINT('Ctrl Pts',(4.97665313471911,2.44905303133571,5.57020641595664));
#18163=CARTESIAN_POINT('Ctrl Pts',(5.05813222715243,2.45024001316067,5.56597921255851));
#18164=CARTESIAN_POINT('Ctrl Pts',(5.13944315623001,2.45142454519341,5.56176073361579));
#18165=CARTESIAN_POINT('Ctrl Pts',(5.22087296166409,2.44855816498041,5.55754225467306));
#18166=CARTESIAN_POINT('Ctrl Pts',(5.3019880106661,2.44164274789679,5.55332377573034));
#18167=CARTESIAN_POINT('Ctrl Pts',(5.38307646017424,2.4347295985378,5.54910668012408));
#18168=CARTESIAN_POINT('Ctrl Pts',(5.46384989557637,2.42377008858651,5.54488958451781));
#18169=CARTESIAN_POINT('Ctrl Pts',(5.54387775932507,2.40881811350597,5.54067248891155));
#18170=CARTESIAN_POINT('Ctrl Pts',(5.62390386690628,2.39386646653832,5.53645548584714));
#18171=CARTESIAN_POINT('Ctrl Pts',(5.70318397879088,2.37492261511099,5.53223848278272));
#18172=CARTESIAN_POINT('Ctrl Pts',(5.78129713029482,2.35209168267122,5.52802147971831));
#18173=CARTESIAN_POINT('Ctrl Pts',(5.85973367184419,2.32916622970402,5.52378701817492));
#18174=CARTESIAN_POINT('Ctrl Pts',(5.93699311348111,2.30232156197441,5.51955255663154));
#18175=CARTESIAN_POINT('Ctrl Pts',(6.01266578101133,2.27171429325571,5.51531809508815));
#18176=CARTESIAN_POINT('Ctrl Pts',(6.08813571400291,2.24118902442819,5.51109497808482));
#18177=CARTESIAN_POINT('Ctrl Pts',(6.16202695742016,2.20692152369236,5.50687186108149));
#18178=CARTESIAN_POINT('Ctrl Pts',(6.23395599308173,2.16911421635828,5.50264874407815));
#18179=CARTESIAN_POINT('Ctrl Pts',(6.30617486270662,2.13115456662692,5.49840861026474));
#18180=CARTESIAN_POINT('Ctrl Pts',(6.37641527654636,2.08962677053247,5.49416847645134));
#18181=CARTESIAN_POINT('Ctrl Pts',(6.44431827901129,2.04477968866833,5.48992834263793));
#18182=CARTESIAN_POINT('Ctrl Pts',(6.51222128147624,1.99993260680418,5.48568820882453));
#18183=CARTESIAN_POINT('Ctrl Pts',(6.57778653276982,1.95176656598373,5.48144807501112));
#18184=CARTESIAN_POINT('Ctrl Pts',(6.64068979568119,1.90056997299931,5.47720794119771));
#18185=CARTESIAN_POINT('Ctrl Pts',(6.70265595672198,1.85013608167508,5.47303097481226));
#18186=CARTESIAN_POINT('Ctrl Pts',(6.76228324590581,1.7965622350999,5.46885400842681));
#18187=CARTESIAN_POINT('Ctrl Pts',(6.81923004557808,1.74009629525162,5.46467704204135));
#18188=CARTESIAN_POINT('Ctrl Pts',(6.8763130790926,1.68349527192215,5.46049008309823));
#18189=CARTESIAN_POINT('Ctrl Pts',(6.93070236814598,1.62398855423778,5.45630312415511));
#18190=CARTESIAN_POINT('Ctrl Pts',(6.98208507709208,1.56186819910249,5.45211616521199));
#18191=CARTESIAN_POINT('Ctrl Pts',(7.03321278119249,1.50005613817553,5.44794998553181));
#18192=CARTESIAN_POINT('Ctrl Pts',(7.08136334922854,1.43565667276068,5.44378380585162));
#18193=CARTESIAN_POINT('Ctrl Pts',(7.12626494788757,1.36899483924671,5.43961762617143));
#18194=CARTESIAN_POINT('Ctrl Pts',(7.17113945057057,1.30237323297402,5.43545396058224));
#18195=CARTESIAN_POINT('Ctrl Pts',(7.21276860737512,1.23349236269166,5.43129029499304));
#18196=CARTESIAN_POINT('Ctrl Pts',(7.25092218098941,1.16270860528618,5.42712662940384));
#18197=CARTESIAN_POINT('Ctrl Pts',(7.28906513501681,1.0919445496856,5.42296412272073));
#18198=CARTESIAN_POINT('Ctrl Pts',(7.32373420028594,1.01927907926535,5.41880161603762));
#18199=CARTESIAN_POINT('Ctrl Pts',(7.35474445735139,0.945094283115184,5.41463910935451));
#18200=CARTESIAN_POINT('Ctrl Pts',(7.38606450716398,0.870168380183887,5.41043501919218));
#18201=CARTESIAN_POINT('Ctrl Pts',(7.41365201386476,0.793693069531089,5.40623092902985));
#18202=CARTESIAN_POINT('Ctrl Pts',(7.43736645441967,0.716082260776893,5.40202683886751));
#18203=CARTESIAN_POINT('Ctrl Pts',(7.46086810650679,0.639167849858436,5.39786047179217));
#18204=CARTESIAN_POINT('Ctrl Pts',(7.48056585136314,0.561138719230343,5.39369410471683));
#18205=CARTESIAN_POINT('Ctrl Pts',(7.4963737850575,0.482410553964754,5.38952773764149));
#18206=CARTESIAN_POINT('Ctrl Pts',(7.5123964108495,0.402613158825711,5.38530478593566));
#18207=CARTESIAN_POINT('Ctrl Pts',(7.52442268876795,0.322098098698098,5.38108183422983));
#18208=CARTESIAN_POINT('Ctrl Pts',(7.53241743836409,0.241304127797563,5.376858882524));
#18209=CARTESIAN_POINT('Ctrl Pts',(7.54041218796023,0.160510156897017,5.37263593081816));
#18210=CARTESIAN_POINT('Ctrl Pts',(7.54437544438211,0.0794377826492872,
5.36841297911234));
#18211=CARTESIAN_POINT('Ctrl Pts',(7.54432671099194,-0.00147590784951311,
5.3641900274065));
#18212=CARTESIAN_POINT('',(7.54432621659511,0.0021450739360106,4.56419002733521));
#18213=CARTESIAN_POINT('Ctrl Pts',(7.54432671099162,-0.00147590839339668,
5.36419002737812));
#18214=CARTESIAN_POINT('Ctrl Pts',(7.54427359039347,-0.0896737956893541,
5.35958690748191));
#18215=CARTESIAN_POINT('Ctrl Pts',(7.53945915089848,-0.177726601365087,
5.35498378758571));
#18216=CARTESIAN_POINT('Ctrl Pts',(7.52992837234614,-0.265256688986924,
5.35038066768951));
#18217=CARTESIAN_POINT('Ctrl Pts',(7.52116581341593,-0.345731494559209,
5.34614857803055));
#18218=CARTESIAN_POINT('Ctrl Pts',(7.50839498671782,-0.42592175353851,5.34191648837158));
#18219=CARTESIAN_POINT('Ctrl Pts',(7.49164371171501,-0.505396886136336,
5.33768439871262));
#18220=CARTESIAN_POINT('Ctrl Pts',(7.47491637828506,-0.584758429787849,
5.33345835772057));
#18221=CARTESIAN_POINT('Ctrl Pts',(7.45421999058225,-0.663406426133667,
5.32923231672851));
#18222=CARTESIAN_POINT('Ctrl Pts',(7.42963408316916,-0.740915816023442,
5.32500627573646));
#18223=CARTESIAN_POINT('Ctrl Pts',(7.40504141320734,-0.818446525485383,
5.32077907233833));
#18224=CARTESIAN_POINT('Ctrl Pts',(7.3765571604242,-0.894837541587461,5.3165518689402));
#18225=CARTESIAN_POINT('Ctrl Pts',(7.34431208924471,-0.969674075541368,
5.31232466554207));
#18226=CARTESIAN_POINT('Ctrl Pts',(7.31213356813603,-1.04435615560664,5.30810618659934));
#18227=CARTESIAN_POINT('Ctrl Pts',(7.2762098978411,-1.11748972697521,5.3038877076566));
#18228=CARTESIAN_POINT('Ctrl Pts',(7.23672016284573,-1.18867985970479,5.29966922871387));
#18229=CARTESIAN_POINT('Ctrl Pts',(7.19724337744447,-1.25984664754935,5.2954521331076));
#18230=CARTESIAN_POINT('Ctrl Pts',(7.15420307488966,-1.32907085632821,5.29123503750133));
#18231=CARTESIAN_POINT('Ctrl Pts',(7.10782455095544,-1.39598164060628,5.28701794189505));
#18232=CARTESIAN_POINT('Ctrl Pts',(7.06144704477249,-1.4628909565639,5.28280093883063));
#18233=CARTESIAN_POINT('Ctrl Pts',(7.01173172852606,-1.52748656769867,5.2785839357662));
#18234=CARTESIAN_POINT('Ctrl Pts',(6.95894672050242,-1.58942733651786,5.27436693270178));
#18235=CARTESIAN_POINT('Ctrl Pts',(6.9059431814658,-1.65162454138703,5.2701324711584));
#18236=CARTESIAN_POINT('Ctrl Pts',(6.84984477555161,-1.71114450746076,5.26589800961503));
#18237=CARTESIAN_POINT('Ctrl Pts',(6.79096198855247,-1.7676774616091,5.26166354807165));
#18238=CARTESIAN_POINT('Ctrl Pts',(6.73223695434608,-1.82405895839863,5.25744043106831));
#18239=CARTESIAN_POINT('Ctrl Pts',(6.67074281927816,-1.87746915230112,5.25321731406496));
#18240=CARTESIAN_POINT('Ctrl Pts',(6.60682117406478,-1.92764087673128,5.24899419706162));
#18241=CARTESIAN_POINT('Ctrl Pts',(6.54264196021344,-1.97801476527473,5.24475406324823));
#18242=CARTESIAN_POINT('Ctrl Pts',(6.4760160218102,-2.02512376565333,5.24051392943484));
#18243=CARTESIAN_POINT('Ctrl Pts',(6.40731727544667,-2.06874211894071,5.23627379562145));
#18244=CARTESIAN_POINT('Ctrl Pts',(6.33861852908312,-2.1123604722281,5.23203366180806));
#18245=CARTESIAN_POINT('Ctrl Pts',(6.26784741197225,-2.15248800203411,5.22779352799467));
#18246=CARTESIAN_POINT('Ctrl Pts',(6.19539972605487,-2.18894680650258,5.22355339418128));
#18247=CARTESIAN_POINT('Ctrl Pts',(6.12308948400112,-2.22533644328286,5.21932130452231));
#18248=CARTESIAN_POINT('Ctrl Pts',(6.04883926109623,-2.25820703877894,5.21508921486335));
#18249=CARTESIAN_POINT('Ctrl Pts',(5.97302558958426,-2.28734788858655,5.21085712520439));
#18250=CARTESIAN_POINT('Ctrl Pts',(5.89732027391621,-2.31644708915979,5.20663108421235));
#18251=CARTESIAN_POINT('Ctrl Pts',(5.82005637780871,-2.34182696605901,5.2024050432203));
#18252=CARTESIAN_POINT('Ctrl Pts',(5.74163391104998,-2.36332322321833,5.19817900222826));
#18253=CARTESIAN_POINT('Ctrl Pts',(5.66318987356985,-2.38482539309364,5.19395179883012));
#18254=CARTESIAN_POINT('Ctrl Pts',(5.58358705627138,-2.40244162072257,5.18972459543199));
#18255=CARTESIAN_POINT('Ctrl Pts',(5.50324469600788,-2.41605619294877,5.18549739203386));
#18256=CARTESIAN_POINT('Ctrl Pts',(5.42306815301737,-2.42964266628376,5.18127891309114));
#18257=CARTESIAN_POINT('Ctrl Pts',(5.34215557068428,-2.43924388332877,5.17706043414842));
#18258=CARTESIAN_POINT('Ctrl Pts',(5.2609357830548,-2.4447954835898,5.1728419552057));
#18259=CARTESIAN_POINT('Ctrl Pts',(5.17974262926538,-2.45034526335317,5.16862485959944));
#18260=CARTESIAN_POINT('Ctrl Pts',(5.09824293348812,-2.45184803188112,5.16440776399318));
#18261=CARTESIAN_POINT('Ctrl Pts',(5.01687043383617,-2.44929130831716,5.16019066838692));
#18262=CARTESIAN_POINT('Ctrl Pts',(4.93549971985906,-2.44673464085909,5.1559736653225));
#18263=CARTESIAN_POINT('Ctrl Pts',(4.85425666088092,-2.4401186741723,5.15175666225809));
#18264=CARTESIAN_POINT('Ctrl Pts',(4.77357333693932,-2.42948301943589,5.14753965919367));
#18265=CARTESIAN_POINT('Ctrl Pts',(4.69255598238572,-2.41880333287126,5.14330519765029));
#18266=CARTESIAN_POINT('Ctrl Pts',(4.61210347681013,-2.4040706530683,5.13907073610691));
#18267=CARTESIAN_POINT('Ctrl Pts',(4.53264460451424,-2.38537720172759,5.13483627456353));
#18268=CARTESIAN_POINT('Ctrl Pts',(4.453398610373,-2.36673383198646,5.1306131575602));
#18269=CARTESIAN_POINT('Ctrl Pts',(4.37514137005613,-2.34415105539881,5.12639004055687));
#18270=CARTESIAN_POINT('Ctrl Pts',(4.29828281380373,-2.31777036189301,5.12216692355353));
#18271=CARTESIAN_POINT('Ctrl Pts',(4.22111456036471,-2.29128336888123,5.11792678974013));
#18272=CARTESIAN_POINT('Ctrl Pts',(4.14535672112182,-2.26096797051504,5.11368665592671));
#18273=CARTESIAN_POINT('Ctrl Pts',(4.07140204223259,-2.22701529807408,5.1094465221133));
#18274=CARTESIAN_POINT('Ctrl Pts',(3.99744736334334,-2.19306262563312,5.10520638829989));
#18275=CARTESIAN_POINT('Ctrl Pts',(3.92529623052259,-2.15547295021282,5.10096625448648));
#18276=CARTESIAN_POINT('Ctrl Pts',(3.85531311721876,-2.11448178689164,5.09672612067307));
#18277=CARTESIAN_POINT('Ctrl Pts',(3.78546277212392,-2.07356838980693,5.09249403101411));
#18278=CARTESIAN_POINT('Ctrl Pts',(3.71751162249781,-2.02911377346407,5.08826194135515));
#18279=CARTESIAN_POINT('Ctrl Pts',(3.65184120019903,-1.98131944795633,5.08402985169619));
#18280=CARTESIAN_POINT('Ctrl Pts',(3.58626463661845,-1.93359343195494,5.07980381070414));
#18281=CARTESIAN_POINT('Ctrl Pts',(3.52296269881731,-1.88253745812472,5.07557776971209));
#18282=CARTESIAN_POINT('Ctrl Pts',(3.46229072743459,-1.8283979692749,5.07135172872005));
#18283=CARTESIAN_POINT('Ctrl Pts',(3.40160206774502,-1.77424358892935,5.06712452532191));
#18284=CARTESIAN_POINT('Ctrl Pts',(3.34354521018652,-1.71700425552863,5.06289732192378));
#18285=CARTESIAN_POINT('Ctrl Pts',(3.28844516845876,-1.65696895898394,5.05867011852565));
#18286=CARTESIAN_POINT('Ctrl Pts',(3.23345884679883,-1.59705756829815,5.05445163958293));
#18287=CARTESIAN_POINT('Ctrl Pts',(3.18141748076258,-1.53436206949927,5.0502331606402));
#18288=CARTESIAN_POINT('Ctrl Pts',(3.13260819768649,-1.46920742228482,5.04601468169748));
#18289=CARTESIAN_POINT('Ctrl Pts',(3.08381492029912,-1.40407414078066,5.04179758609121));
#18290=CARTESIAN_POINT('Ctrl Pts',(3.03825189944845,-1.33648368393946,5.03758049048495));
#18291=CARTESIAN_POINT('Ctrl Pts',(2.99616538269492,-1.26679332849086,5.03336339487868));
#18292=CARTESIAN_POINT('Ctrl Pts',(2.95407978950688,-1.19710450235885,5.02914639181427));
#18293=CARTESIAN_POINT('Ctrl Pts',(2.91547078796979,-1.12531626761495,5.02492938874985));
#18294=CARTESIAN_POINT('Ctrl Pts',(2.88054000053615,-1.05181282549681,5.02071238568544));
#18295=CARTESIAN_POINT('Ctrl Pts',(2.84546459892786,-0.97800507762445,5.01647792414205));
#18296=CARTESIAN_POINT('Ctrl Pts',(2.81409814620316,-0.902468310742165,
5.01224346259867));
#18297=CARTESIAN_POINT('Ctrl Pts',(2.78659631431143,-0.825612557853047,
5.00800900105529));
#18298=CARTESIAN_POINT('Ctrl Pts',(2.75916816253937,-0.74896270910489,5.00378588405195));
#18299=CARTESIAN_POINT('Ctrl Pts',(2.73558404662131,-0.671001392179162,
4.99956276704862));
#18300=CARTESIAN_POINT('Ctrl Pts',(2.71594803617518,-0.592149596049849,
4.99533965004528));
#18301=CARTESIAN_POINT('Ctrl Pts',(2.69623290354037,-0.512980071087197,
4.99109951623188));
#18302=CARTESIAN_POINT('Ctrl Pts',(2.6804978433303,-0.432913339762491,4.98685938241847));
#18303=CARTESIAN_POINT('Ctrl Pts',(2.66879591741602,-0.352382951551732,
4.98261924860506));
#18304=CARTESIAN_POINT('Ctrl Pts',(2.65709399150175,-0.271852563340974,
4.97837911479166));
#18305=CARTESIAN_POINT('Ctrl Pts',(2.64942518200459,-0.190858989358832,
4.97413898097825));
#18306=CARTESIAN_POINT('Ctrl Pts',(2.64578992844837,-0.109836174364002,
4.96989884716485));
#18307=CARTESIAN_POINT('Ctrl Pts',(2.64216157150021,-0.028967071507964,
4.96566675750589));
#18308=CARTESIAN_POINT('Ctrl Pts',(2.6425379274089,0.0522328669521893,4.96143466784692));
#18309=CARTESIAN_POINT('Ctrl Pts',(2.6469572506401,0.133333862616992,4.95720257818796));
#18310=CARTESIAN_POINT('Ctrl Pts',(2.65137025760289,0.214318945588814,4.95297653719591));
#18311=CARTESIAN_POINT('Ctrl Pts',(2.65981473035323,0.295204906503583,4.94875049620386));
#18312=CARTESIAN_POINT('Ctrl Pts',(2.67227697172965,0.37555952618575,4.94452445521182));
#18313=CARTESIAN_POINT('Ctrl Pts',(2.68474264094438,0.455936248043244,4.94029725181368));
#18314=CARTESIAN_POINT('Ctrl Pts',(2.70122828366823,0.535780869538422,4.93607004841555));
#18315=CARTESIAN_POINT('Ctrl Pts',(2.72166800539681,0.614663498838341,4.93184284501742));
#18316=CARTESIAN_POINT('Ctrl Pts',(2.74206554192066,0.693383323580008,4.92762436607469));
#18317=CARTESIAN_POINT('Ctrl Pts',(2.76640075986749,0.771144666907163,4.92340588713197));
#18318=CARTESIAN_POINT('Ctrl Pts',(2.79455697894836,0.847529884685964,4.91918740818925));
#18319=CARTESIAN_POINT('Ctrl Pts',(2.82270396495613,0.923890053991553,4.91497031258298));
#18320=CARTESIAN_POINT('Ctrl Pts',(2.85466930317231,0.998874558242534,4.91075321697672));
#18321=CARTESIAN_POINT('Ctrl Pts',(2.89028696632642,1.0720824991126,4.90653612137046));
#18322=CARTESIAN_POINT('Ctrl Pts',(2.92590384787049,1.14528883347462,4.90231911830604));
#18323=CARTESIAN_POINT('Ctrl Pts',(2.96517269066395,1.21671826461475,4.89810211524162));
#18324=CARTESIAN_POINT('Ctrl Pts',(3.00788061081709,1.28599271495644,4.89388511217721));
#18325=CARTESIAN_POINT('Ctrl Pts',(3.05076534263344,1.35555396293986,4.88965065063383));
#18326=CARTESIAN_POINT('Ctrl Pts',(3.09711745153464,1.42294194041336,4.88541618909044));
#18327=CARTESIAN_POINT('Ctrl Pts',(3.14667739375347,1.48780309702361,4.88118172754706));
#18328=CARTESIAN_POINT('Ctrl Pts',(3.19610455999986,1.55249048419915,4.87695861054373));
#18329=CARTESIAN_POINT('Ctrl Pts',(3.24872205982467,1.61466424210887,4.8727354935404));
#18330=CARTESIAN_POINT('Ctrl Pts',(3.30423310345936,1.67400817771856,4.86851237653707));
#18331=CARTESIAN_POINT('Ctrl Pts',(3.35996782569106,1.73359123634573,4.86427224272366));
#18332=CARTESIAN_POINT('Ctrl Pts',(3.41861911483818,1.79032129774366,4.86003210891026));
#18333=CARTESIAN_POINT('Ctrl Pts',(3.47985191156125,1.84391815493645,4.85579197509685));
#18334=CARTESIAN_POINT('Ctrl Pts',(3.54108470828434,1.89751501212924,4.85155184128345));
#18335=CARTESIAN_POINT('Ctrl Pts',(3.60489860743153,1.94797842403463,4.84731170747004));
#18336=CARTESIAN_POINT('Ctrl Pts',(3.67092961338773,1.99507213773946,4.84307157365664));
#18337=CARTESIAN_POINT('Ctrl Pts',(3.73683534886111,2.0420765077766,4.83883948399768));
#18338=CARTESIAN_POINT('Ctrl Pts',(3.80519565810399,2.08589933025432,4.83460739433872));
#18339=CARTESIAN_POINT('Ctrl Pts',(3.87567059803625,2.12627487677918,4.83037530467976));
#18340=CARTESIAN_POINT('Ctrl Pts',(3.9460448124471,2.16659271700475,4.82614926368771));
#18341=CARTESIAN_POINT('Ctrl Pts',(4.01852725507035,2.20347283772712,4.82192322269567));
#18342=CARTESIAN_POINT('Ctrl Pts',(4.09274769424177,2.23669178975129,4.81769718170362));
#18343=CARTESIAN_POINT('Ctrl Pts',(4.16698854833357,2.26991987891164,4.81346997830549));
#18344=CARTESIAN_POINT('Ctrl Pts',(4.24296796032465,2.29948453604171,4.80924277490735));
#18345=CARTESIAN_POINT('Ctrl Pts',(4.32028927855363,2.32520738924549,4.80501557150922));
#18346=CARTESIAN_POINT('Ctrl Pts',(4.3974510145885,2.35087715347657,4.8007970925665));
#18347=CARTESIAN_POINT('Ctrl Pts',(4.47594869025038,2.37272078559757,4.79657861362378));
#18348=CARTESIAN_POINT('Ctrl Pts',(4.55536832789648,2.39060919872453,4.79236013468106));
#18349=CARTESIAN_POINT('Ctrl Pts',(4.63476192201317,2.40849174582859,4.78814303907479));
#18350=CARTESIAN_POINT('Ctrl Pts',(4.71507642472783,2.42242154764815,4.78392594346853));
#18351=CARTESIAN_POINT('Ctrl Pts',(4.79588509004013,2.43232003972698,4.77970884786227));
#18352=CARTESIAN_POINT('Ctrl Pts',(4.87669198205068,2.44221831458884,4.77549184479785));
#18353=CARTESIAN_POINT('Ctrl Pts',(4.95799255371693,2.44808540024345,4.77127484173343));
#18354=CARTESIAN_POINT('Ctrl Pts',(5.03935374343865,2.44989446658086,4.76705783866902));
#18355=CARTESIAN_POINT('Ctrl Pts',(5.12105177015047,2.45171102248992,4.76282337712563));
#18356=CARTESIAN_POINT('Ctrl Pts',(5.20281044650648,2.44943586357772,4.75858891558225));
#18357=CARTESIAN_POINT('Ctrl Pts',(5.28419193459185,2.44309465655006,4.75435445403887));
#18358=CARTESIAN_POINT('Ctrl Pts',(5.36535539364532,2.43677043824136,4.75013133703554));
#18359=CARTESIAN_POINT('Ctrl Pts',(5.44614322436611,2.426402031042,4.7459082200322));
#18360=CARTESIAN_POINT('Ctrl Pts',(5.52612869875587,2.41206667106406,4.74168510302887));
#18361=CARTESIAN_POINT('Ctrl Pts',(5.60643647007122,2.39767354756739,4.73744496921546));
#18362=CARTESIAN_POINT('Ctrl Pts',(5.68593494793438,2.37928154924516,4.73320483540205));
#18363=CARTESIAN_POINT('Ctrl Pts',(5.76420680689355,2.357019595365,4.72896470158864));
#18364=CARTESIAN_POINT('Ctrl Pts',(5.84247866585271,2.33475764148485,4.72472456777523));
#18365=CARTESIAN_POINT('Ctrl Pts',(5.9195234833211,2.30862594106612,4.72048443396183));
#18366=CARTESIAN_POINT('Ctrl Pts',(5.99494509779219,2.27880159381956,4.71624430014842));
#18367=CARTESIAN_POINT('Ctrl Pts',(6.07022362642167,2.24903382772493,4.71201221048946));
#18368=CARTESIAN_POINT('Ctrl Pts',(6.14416596005128,2.21547637032556,4.70778012083049));
#18369=CARTESIAN_POINT('Ctrl Pts',(6.21636427122028,2.17827011036857,4.70354803117153));
#18370=CARTESIAN_POINT('Ctrl Pts',(6.28845939375883,2.14111702704338,4.69932199017948));
#18371=CARTESIAN_POINT('Ctrl Pts',(6.35881503484589,2.10032570982544,4.69509594918743));
#18372=CARTESIAN_POINT('Ctrl Pts',(6.42704239006832,2.05608545255053,4.69086990819538));
#18373=CARTESIAN_POINT('Ctrl Pts',(6.49528851176577,2.01183302664207,4.68664270479725));
#18374=CARTESIAN_POINT('Ctrl Pts',(6.56140475299479,1.96412995919908,4.68241550139911));
#18375=CARTESIAN_POINT('Ctrl Pts',(6.6250257838841,1.91321222301423,4.67818829800098));
#18376=CARTESIAN_POINT('Ctrl Pts',(6.68851550837652,1.86239957510574,4.67396981905826));
#18377=CARTESIAN_POINT('Ctrl Pts',(6.74951993344191,1.80838578546829,4.66975134011554));
#18378=CARTESIAN_POINT('Ctrl Pts',(6.80770567885527,1.75144815995816,4.66553286117281));
#18379=CARTESIAN_POINT('Ctrl Pts',(6.86587234382183,1.69452920560756,4.66131576556655));
#18380=CARTESIAN_POINT('Ctrl Pts',(6.92122183286112,1.63468864421207,4.65709866996029));
#18381=CARTESIAN_POINT('Ctrl Pts',(6.97345623146422,1.57224196185371,4.65288157435402));
#18382=CARTESIAN_POINT('Ctrl Pts',(7.02568948381219,1.50979664985344,4.6486645712896));
#18383=CARTESIAN_POINT('Ctrl Pts',(7.07480748437667,1.44474568777064,4.64444756822518));
#18384=CARTESIAN_POINT('Ctrl Pts',(7.12055230919156,1.37743798452194,4.64023056516076));
#18385=CARTESIAN_POINT('Ctrl Pts',(7.16648651851705,1.30985162600478,4.63599610361738));
#18386=CARTESIAN_POINT('Ctrl Pts',(7.2090192867098,1.23999018358184,4.631761642074));
#18387=CARTESIAN_POINT('Ctrl Pts',(7.24793415705635,1.16823511145826,4.62752718053062));
#18388=CARTESIAN_POINT('Ctrl Pts',(7.28674477062775,1.09667227824884,4.62330406352729));
#18389=CARTESIAN_POINT('Ctrl Pts',(7.32195668199649,1.02322638824681,4.61908094652395));
#18390=CARTESIAN_POINT('Ctrl Pts',(7.35340275872277,0.948297602606147,4.61485782952062));
#18391=CARTESIAN_POINT('Ctrl Pts',(7.3849755456289,0.873066895680105,4.61061769570722));
#18392=CARTESIAN_POINT('Ctrl Pts',(7.4127519330167,0.79634176362735,4.60637756189381));
#18393=CARTESIAN_POINT('Ctrl Pts',(7.43661328010294,0.718542569475346,4.60213742808041));
#18394=CARTESIAN_POINT('Ctrl Pts',(7.46047462718918,0.640743375323342,4.597897294267));
#18395=CARTESIAN_POINT('Ctrl Pts',(7.48042087970568,0.561870587392111,4.5936571604536));
#18396=CARTESIAN_POINT('Ctrl Pts',(7.49638534176927,0.482352994564379,4.5894170266402));
#18397=CARTESIAN_POINT('Ctrl Pts',(7.51922595399674,0.368585897633325,4.58335059910642));
#18398=CARTESIAN_POINT('Ctrl Pts',(7.53399165590837,0.253147670596884,4.57728417157264));
#18399=CARTESIAN_POINT('Ctrl Pts',(7.54049542395804,0.136984064369133,4.57121774403885));
#18400=CARTESIAN_POINT('Ctrl Pts',(7.54300687674887,0.0921270813362655,
4.5688751718186));
#18401=CARTESIAN_POINT('Ctrl Pts',(7.54428681030233,0.047162191867149,4.56653259959836));
#18402=CARTESIAN_POINT('Ctrl Pts',(7.54432621659438,0.00214507476044559,
4.56419002737811));
#18403=CARTESIAN_POINT('',(7.54393144410385,-8.94937127778141E-5,3.76419002093224));
#18404=CARTESIAN_POINT('Ctrl Pts',(7.54432621659511,0.00214507393599264,
4.56419002733521));
#18405=CARTESIAN_POINT('Ctrl Pts',(7.5443974290659,-0.0792069437733646,
4.55995668257674));
#18406=CARTESIAN_POINT('Ctrl Pts',(7.54041302387128,-0.160689976853086,
4.55572333781828));
#18407=CARTESIAN_POINT('Ctrl Pts',(7.53236234262211,-0.24186027151777,4.55148999305981));
#18408=CARTESIAN_POINT('Ctrl Pts',(7.52445196900467,-0.321615926668248,
4.54733042722253));
#18409=CARTESIAN_POINT('Ctrl Pts',(7.51261596087068,-0.401069158613352,
4.54317086138524));
#18410=CARTESIAN_POINT('Ctrl Pts',(7.49689665975842,-0.479799132427131,
4.53901129554796));
#18411=CARTESIAN_POINT('Ctrl Pts',(7.48118511182865,-0.558490274498342,
4.53485378132053));
#18412=CARTESIAN_POINT('Ctrl Pts',(7.46159416428309,-0.636458396846393,
4.53069626709309));
#18413=CARTESIAN_POINT('Ctrl Pts',(7.43821764561932,-0.713290599698506,
4.52653875286566));
#18414=CARTESIAN_POINT('Ctrl Pts',(7.4148450175322,-0.79011001529264,4.52238193057735));
#18415=CARTESIAN_POINT('Ctrl Pts',(7.38768820935881,-0.865793428407507,
4.51822510828904));
#18416=CARTESIAN_POINT('Ctrl Pts',(7.35689109022829,-0.939942486070237,
4.51406828600073));
#18417=CARTESIAN_POINT('Ctrl Pts',(7.3251081881406,-1.01646497603433,4.50977840826167));
#18418=CARTESIAN_POINT('Ctrl Pts',(7.28944814638986,-1.09135270273389,4.5054885305226));
#18419=CARTESIAN_POINT('Ctrl Pts',(7.25012225160305,-1.16419143972103,4.50119865278354));
#18420=CARTESIAN_POINT('Ctrl Pts',(7.21196864925899,-1.23485887707538,4.49703665493841));
#18421=CARTESIAN_POINT('Ctrl Pts',(7.17036499723818,-1.30359738498881,4.49287465709327));
#18422=CARTESIAN_POINT('Ctrl Pts',(7.12554925654193,-1.37005677033736,4.48871265924813));
#18423=CARTESIAN_POINT('Ctrl Pts',(7.07866802985326,-1.43957916273142,4.48435884156211));
#18424=CARTESIAN_POINT('Ctrl Pts',(7.0282718432639,-1.50660680265638,4.48000502387608));
#18425=CARTESIAN_POINT('Ctrl Pts',(6.97467977651927,-1.57077804537387,4.47565120619006));
#18426=CARTESIAN_POINT('Ctrl Pts',(6.92108770977463,-1.63494928809137,4.47129738850404));
#18427=CARTESIAN_POINT('Ctrl Pts',(6.86430022451696,-1.69626375536162,4.46694357081801));
#18428=CARTESIAN_POINT('Ctrl Pts',(6.80467773584324,-1.75440603669126,4.46258975313199));
#18429=CARTESIAN_POINT('Ctrl Pts',(6.7467222273782,-1.81092272280642,4.45835766347302));
#18430=CARTESIAN_POINT('Ctrl Pts',(6.68585512058094,-1.86466997352523,4.45412557381406));
#18431=CARTESIAN_POINT('Ctrl Pts',(6.62237179651123,-1.91533326872701,4.4498934841551));
#18432=CARTESIAN_POINT('Ctrl Pts',(6.5589792052739,-1.96592415397959,4.44566744316305));
#18433=CARTESIAN_POINT('Ctrl Pts',(6.49297818338994,-2.01343955046774,4.44144140217099));
#18434=CARTESIAN_POINT('Ctrl Pts',(6.42470050116979,-2.05760209653395,4.43721536117894));
#18435=CARTESIAN_POINT('Ctrl Pts',(6.35640403863182,-2.10177678985858,4.43298815778081));
#18436=CARTESIAN_POINT('Ctrl Pts',(6.28583001538824,-2.14259648168666,4.42876095438268));
#18437=CARTESIAN_POINT('Ctrl Pts',(6.21334319503714,-2.17982432482852,4.42453375098454));
#18438=CARTESIAN_POINT('Ctrl Pts',(6.14100597903965,-2.21697533403859,4.42031527204182));
#18439=CARTESIAN_POINT('Ctrl Pts',(6.06676425559604,-2.25054907152311,4.4160967930991));
#18440=CARTESIAN_POINT('Ctrl Pts',(5.99100743671944,-2.28035475154785,4.41187831415638));
#18441=CARTESIAN_POINT('Ctrl Pts',(5.91527546024961,-2.31015065760323,4.40766121855012));
#18442=CARTESIAN_POINT('Ctrl Pts',(5.83802980710514,-2.33618079005223,4.40344412294386));
#18443=CARTESIAN_POINT('Ctrl Pts',(5.75968022248452,-2.35830234345066,4.3992270273376));
#18444=CARTESIAN_POINT('Ctrl Pts',(5.68133235720239,-2.38042341140378,4.39501002427318));
#18445=CARTESIAN_POINT('Ctrl Pts',(5.60188105612765,-2.39863594568316,4.39079302120876));
#18446=CARTESIAN_POINT('Ctrl Pts',(5.52175020561123,-2.41284730414989,4.38657601814434));
#18447=CARTESIAN_POINT('Ctrl Pts',(5.44128761173427,-2.42711749793142,4.38234155660096));
#18448=CARTESIAN_POINT('Ctrl Pts',(5.36014029203761,-2.43735322035853,4.37810709505758));
#18449=CARTESIAN_POINT('Ctrl Pts',(5.27874486921592,-2.44351298116804,4.3738726335142));
#18450=CARTESIAN_POINT('Ctrl Pts',(5.19756751275862,-2.44965623937092,4.36964951651086));
#18451=CARTESIAN_POINT('Ctrl Pts',(5.11614384934172,-2.45174537703917,4.36542639950753));
#18452=CARTESIAN_POINT('Ctrl Pts',(5.03490739645501,-2.44979156501111,4.36120328250419));
#18453=CARTESIAN_POINT('Ctrl Pts',(4.95334360589602,-2.44782988020848,4.35696314869079));
#18454=CARTESIAN_POINT('Ctrl Pts',(4.87196900727807,-2.44179263873569,4.35272301487739));
#18455=CARTESIAN_POINT('Ctrl Pts',(4.79121571760313,-2.43174352423983,4.34848288106398));
#18456=CARTESIAN_POINT('Ctrl Pts',(4.7104624279282,-2.42169440974398,4.34424274725058));
#18457=CARTESIAN_POINT('Ctrl Pts',(4.63033089674386,-2.40763356426609,4.34000261343717));
#18458=CARTESIAN_POINT('Ctrl Pts',(4.55123968223925,-2.38967551854041,4.33576247962377));
#18459=CARTESIAN_POINT('Ctrl Pts',(4.47229851534452,-2.37175154185586,4.3315303899648));
#18460=CARTESIAN_POINT('Ctrl Pts',(4.39409920452606,-2.34987828336003,4.32729830030584));
#18461=CARTESIAN_POINT('Ctrl Pts',(4.3170663078638,-2.32413270611907,4.32306621064687));
#18462=CARTESIAN_POINT('Ctrl Pts',(4.24014350960956,-2.29842392545711,4.31884016965483));
#18463=CARTESIAN_POINT('Ctrl Pts',(4.16438425154372,-2.26885396417153,4.31461412866279));
#18464=CARTESIAN_POINT('Ctrl Pts',(4.09020168302774,-2.23555052752089,4.31038808767075));
#18465=CARTESIAN_POINT('Ctrl Pts',(4.01599871000794,-2.20223793049588,4.30616088427261));
#18466=CARTESIAN_POINT('Ctrl Pts',(3.94337374263392,-2.16518993309185,4.30193368087448));
#18467=CARTESIAN_POINT('Ctrl Pts',(3.87272385868301,-2.12458395659414,4.29770647747635));
#18468=CARTESIAN_POINT('Ctrl Pts',(3.802219787863,-2.08406178610197,4.29348799853363));
#18469=CARTESIAN_POINT('Ctrl Pts',(3.73368307129339,-2.0399965182552,4.28926951959091));
#18470=CARTESIAN_POINT('Ctrl Pts',(3.6674855231533,-1.99261130127486,4.28505104064819));
#18471=CARTESIAN_POINT('Ctrl Pts',(3.60130968271473,-1.94524162299914,4.28083394504193));
#18472=CARTESIAN_POINT('Ctrl Pts',(3.53747186494722,-1.8945544278931,4.27661684943566));
#18473=CARTESIAN_POINT('Ctrl Pts',(3.47631466416907,-1.84081601213703,4.2723997538294));
#18474=CARTESIAN_POINT('Ctrl Pts',(3.41515880545205,-1.78707877564095,4.26818275076498));
#18475=CARTESIAN_POINT('Ctrl Pts',(3.35668379508103,-1.73029075921625,4.26396574770056));
#18476=CARTESIAN_POINT('Ctrl Pts',(3.30119780931492,-1.67075739632185,4.25974874463614));
#18477=CARTESIAN_POINT('Ctrl Pts',(3.24548211043251,-1.61097756408703,4.25551428309276));
#18478=CARTESIAN_POINT('Ctrl Pts',(3.1927805692189,-1.54842994173995,4.25127982154938));
#18479=CARTESIAN_POINT('Ctrl Pts',(3.14336535048328,-1.48345845825012,4.247045360006));
#18480=CARTESIAN_POINT('Ctrl Pts',(3.09408251999165,-1.41866103977161,4.24282224300266));
#18481=CARTESIAN_POINT('Ctrl Pts',(3.04806865587497,-1.35145314016538,4.23859912599933));
#18482=CARTESIAN_POINT('Ctrl Pts',(3.00555003355359,-1.28220470758419,4.23437600899599));
#18483=CARTESIAN_POINT('Ctrl Pts',(2.96286008485882,-1.21267724237755,4.23013587518259));
#18484=CARTESIAN_POINT('Ctrl Pts',(2.92369382390486,-1.14109318278515,4.22589574136918));
#18485=CARTESIAN_POINT('Ctrl Pts',(2.88823268784501,-1.06784984640001,4.22165560755577));
#18486=CARTESIAN_POINT('Ctrl Pts',(2.85277155178516,-0.994606510014861,
4.21741547374237));
#18487=CARTESIAN_POINT('Ctrl Pts',(2.82101566576168,-0.919704351378593,
4.21317533992896));
#18488=CARTESIAN_POINT('Ctrl Pts',(2.79309641776494,-0.843556946896196,
4.20893520611555));
#18489=CARTESIAN_POINT('Ctrl Pts',(2.76523013666801,-0.767554005185311,
4.20470311645659));
#18490=CARTESIAN_POINT('Ctrl Pts',(2.74108197119417,-0.690026992125681,
4.20047102679762));
#18491=CARTESIAN_POINT('Ctrl Pts',(2.72081810344044,-0.611374099112766,
4.19623893713866));
#18492=CARTESIAN_POINT('Ctrl Pts',(2.70058319759358,-0.532833619869503,
4.19201289614662));
#18493=CARTESIAN_POINT('Ctrl Pts',(2.68422167837414,-0.453170902856112,
4.18778685515458));
#18494=CARTESIAN_POINT('Ctrl Pts',(2.67185093551015,-0.372802145957868,
4.18356081416254));
#18495=CARTESIAN_POINT('Ctrl Pts',(2.65947678997521,-0.292411282995653,
4.1793336107644));
#18496=CARTESIAN_POINT('Ctrl Pts',(2.65109575197383,-0.211314438422341,
4.17510640736627));
#18497=CARTESIAN_POINT('Ctrl Pts',(2.64677474554044,-0.129941345000655,
4.17087920396814));
#18498=CARTESIAN_POINT('Ctrl Pts',(2.642462657161,-0.0487361961651143,4.16666072502541));
#18499=CARTESIAN_POINT('Ctrl Pts',(2.64219390782991,0.0327435996271821,
4.16244224608269));
#18500=CARTESIAN_POINT('Ctrl Pts',(2.64598330755776,0.114064658509501,4.15822376713997));
#18501=CARTESIAN_POINT('Ctrl Pts',(2.64977146465412,0.195359050342644,4.15400667153371));
#18502=CARTESIAN_POINT('Ctrl Pts',(2.6576151064267,0.276494344812994,4.14978957592744));
#18503=CARTESIAN_POINT('Ctrl Pts',(2.66947694299592,0.357038229548013,4.14557248032117));
#18504=CARTESIAN_POINT('Ctrl Pts',(2.68133851926364,0.437580346791695,4.14135547725675));
#18505=CARTESIAN_POINT('Ctrl Pts',(2.69721804616645,0.517530620541599,4.13713847419234));
#18506=CARTESIAN_POINT('Ctrl Pts',(2.7170266746867,0.596464353191837,4.13292147112792));
#18507=CARTESIAN_POINT('Ctrl Pts',(2.73691731133429,0.675724873110183,4.12868700958454));
#18508=CARTESIAN_POINT('Ctrl Pts',(2.76076954967425,0.753959956248967,4.12445254804115));
#18509=CARTESIAN_POINT('Ctrl Pts',(2.78844265408706,0.830754206044847,4.12021808649777));
#18510=CARTESIAN_POINT('Ctrl Pts',(2.81604161952421,0.907342716472562,4.11599496949444));
#18511=CARTESIAN_POINT('Ctrl Pts',(2.84744078598348,0.982497688404455,4.11177185249111));
#18512=CARTESIAN_POINT('Ctrl Pts',(2.88245263387798,1.05582809932695,4.10754873548778));
#18513=CARTESIAN_POINT('Ctrl Pts',(2.91760556002476,1.12945399097481,4.10330860167437));
#18514=CARTESIAN_POINT('Ctrl Pts',(2.95640011152989,1.20124017598528,4.09906846786097));
#18515=CARTESIAN_POINT('Ctrl Pts',(2.99860142286109,1.27081838965457,4.09482833404756));
#18516=CARTESIAN_POINT('Ctrl Pts',(3.04080273419228,1.34039660332386,4.09058820023415));
#18517=CARTESIAN_POINT('Ctrl Pts',(3.08641049185181,1.4077664935329,4.08634806642074));
#18518=CARTESIAN_POINT('Ctrl Pts',(3.13514897760213,1.47259296671225,4.08210793260734));
#18519=CARTESIAN_POINT('Ctrl Pts',(3.18379499931147,1.53729645458376,4.07787584294837));
#18520=CARTESIAN_POINT('Ctrl Pts',(3.23574135673275,1.59970757218604,4.07364375328941));
#18521=CARTESIAN_POINT('Ctrl Pts',(3.29074415854736,1.65947038427004,4.06941166363045));
#18522=CARTESIAN_POINT('Ctrl Pts',(3.34566834822134,1.71914778102187,4.06518562263839));
#18523=CARTESIAN_POINT('Ctrl Pts',(3.40363999413768,1.77618405073598,4.06095958164635));
#18524=CARTESIAN_POINT('Ctrl Pts',(3.464373568516,1.83025442439509,4.0567335406543));
#18525=CARTESIAN_POINT('Ctrl Pts',(3.52512384814549,1.88433967053916,4.05250633725616));
#18526=CARTESIAN_POINT('Ctrl Pts',(3.58863727450789,1.9354570322613,4.04827913385803));
#18527=CARTESIAN_POINT('Ctrl Pts',(3.6545895270529,1.98331674197465,4.04405193045989));
#18528=CARTESIAN_POINT('Ctrl Pts',(3.72040566183107,2.03107767482206,4.03983345151717));
#18529=CARTESIAN_POINT('Ctrl Pts',(3.78865020450153,2.07559409588503,4.03561497257445));
#18530=CARTESIAN_POINT('Ctrl Pts',(3.85896744175701,2.11661799517305,4.03139649363173));
#18531=CARTESIAN_POINT('Ctrl Pts',(3.92926162036989,2.15762844177908,4.02717939802547));
#18532=CARTESIAN_POINT('Ctrl Pts',(4.00162674271221,2.19514840704304,4.02296230241921));
#18533=CARTESIAN_POINT('Ctrl Pts',(4.07567967434793,2.22897419382082,4.01874520681295));
#18534=CARTESIAN_POINT('Ctrl Pts',(4.14973098093263,2.26279923831024,4.01452820374855));
#18535=CARTESIAN_POINT('Ctrl Pts',(4.22546960001108,2.29293007346946,4.01031120068414));
#18536=CARTESIAN_POINT('Ctrl Pts',(4.30249076210192,2.31921041791338,4.00609419761973));
#18537=CARTESIAN_POINT('Ctrl Pts',(4.3798307933799,2.34559956352106,4.00185973607635));
#18538=CARTESIAN_POINT('Ctrl Pts',(4.45846356743338,2.36810610373105,3.99762527453296));
#18539=CARTESIAN_POINT('Ctrl Pts',(4.53796391711992,2.38662236440325,3.99339081298958));
#18540=CARTESIAN_POINT('Ctrl Pts',(4.61725127752986,2.40508901818715,3.98916769598624));
#18541=CARTESIAN_POINT('Ctrl Pts',(4.69740110343043,2.41958670312448,3.98494457898291));
#18542=CARTESIAN_POINT('Ctrl Pts',(4.77798325534455,2.43006026278449,3.98072146197957));
#18543=CARTESIAN_POINT('Ctrl Pts',(4.85889010846239,2.44057602505821,3.97648132816616));
#18544=CARTESIAN_POINT('Ctrl Pts',(4.94023230836427,2.44703513490167,3.97224119435275));
#18545=CARTESIAN_POINT('Ctrl Pts',(5.02157308115586,2.44943454673675,3.96800106053934));
#18546=CARTESIAN_POINT('Ctrl Pts',(5.10291385394746,2.45183395857182,3.96376092672594));
#18547=CARTESIAN_POINT('Ctrl Pts',(5.18425273366386,2.45017374412987,3.95952079291253));
#18548=CARTESIAN_POINT('Ctrl Pts',(5.26515858208946,2.44450317902161,3.95528065909912));
#18549=CARTESIAN_POINT('Ctrl Pts',(5.34591094027888,2.43884337180533,3.95104856944016));
#18550=CARTESIAN_POINT('Ctrl Pts',(5.42653318044006,2.42916731676783,3.9468164797812));
#18551=CARTESIAN_POINT('Ctrl Pts',(5.50659397124849,2.41548624624073,3.94258439012223));
#18552=CARTESIAN_POINT('Ctrl Pts',(5.58654033606508,2.40182472923101,3.93835834913019));
#18553=CARTESIAN_POINT('Ctrl Pts',(5.66592639105077,2.38416964308183,3.93413230813815));
#18554=CARTESIAN_POINT('Ctrl Pts',(5.74432433169595,2.36258410933877,3.9299062671461));
#18555=CARTESIAN_POINT('Ctrl Pts',(5.82274383631645,2.34099263832347,3.92567906374797));
#18556=CARTESIAN_POINT('Ctrl Pts',(5.90017421987549,2.31546861631226,3.92145186034983));
#18557=CARTESIAN_POINT('Ctrl Pts',(5.97619596955491,2.28612675193231,3.9172246569517));
#18558=CARTESIAN_POINT('Ctrl Pts',(6.05206081919822,2.25684544574262,3.91300617800898));
#18559=CARTESIAN_POINT('Ctrl Pts',(6.12652240111848,2.22376218462051,3.90878769906627));
#18560=CARTESIAN_POINT('Ctrl Pts',(6.19917918752775,2.1870407255441,3.90456922012355));
#18561=CARTESIAN_POINT('Ctrl Pts',(6.27181214810243,2.15033130828035,3.90035212451729));
#18562=CARTESIAN_POINT('Ctrl Pts',(6.34264107408625,2.10998627179495,3.89613502891103));
#18563=CARTESIAN_POINT('Ctrl Pts',(6.41128672638872,2.06621647678798,3.89191793330477));
#18564=CARTESIAN_POINT('Ctrl Pts',(6.47993087230028,2.022447642285,3.88770093024034));
#18565=CARTESIAN_POINT('Ctrl Pts',(6.54639144859062,1.97525444948642,3.88348392717592));
#18566=CARTESIAN_POINT('Ctrl Pts',(6.61031725452114,1.92489169290863,3.87926692411149));
#18567=CARTESIAN_POINT('Ctrl Pts',(6.67450771459596,1.87432043348831,3.87503246256811));
#18568=CARTESIAN_POINT('Ctrl Pts',(6.73614199302478,1.82055359212562,3.87079800102473));
#18569=CARTESIAN_POINT('Ctrl Pts',(6.79489860012106,1.76388950621497,3.86656353948135));
#18570=CARTESIAN_POINT('Ctrl Pts',(6.85349779247285,1.70737722897821,3.86234042247801));
#18571=CARTESIAN_POINT('Ctrl Pts',(6.90923442299321,1.6479835805073,3.85811730547466));
#18572=CARTESIAN_POINT('Ctrl Pts',(6.96182838023272,1.58603961937333,3.85389418847132));
#18573=CARTESIAN_POINT('Ctrl Pts',(7.01463426183523,1.5238460585668,3.84965405465792));
#18574=CARTESIAN_POINT('Ctrl Pts',(7.06427181029886,1.45908196846006,3.84541392084452));
#18575=CARTESIAN_POINT('Ctrl Pts',(7.11050104743721,1.39211230272191,3.84117378703111));
#18576=CARTESIAN_POINT('Ctrl Pts',(7.15673028457556,1.32514263698376,3.83693365321771));
#18577=CARTESIAN_POINT('Ctrl Pts',(7.19955101730732,1.25596782571684,3.8326935194043));
#18578=CARTESIAN_POINT('Ctrl Pts',(7.23877024704368,1.18497653303256,3.8284533855909));
#18579=CARTESIAN_POINT('Ctrl Pts',(7.27979763224546,1.11071227209453,3.82401776550252));
#18580=CARTESIAN_POINT('Ctrl Pts',(7.31702493902606,1.03420556025212,3.81958214541413));
#18581=CARTESIAN_POINT('Ctrl Pts',(7.35021345270098,0.95586145836729,3.81514652532574));
#18582=CARTESIAN_POINT('Ctrl Pts',(7.38331144713044,0.877731034294547,3.81072300306697));
#18583=CARTESIAN_POINT('Ctrl Pts',(7.41239243550678,0.797773568689021,3.8062994808082));
#18584=CARTESIAN_POINT('Ctrl Pts',(7.43726394308882,0.716417666138689,3.80187595854942));
#18585=CARTESIAN_POINT('Ctrl Pts',(7.46209503840555,0.635193954060035,3.79745962381455));
#18586=CARTESIAN_POINT('Ctrl Pts',(7.4827301416554,0.552576704787212,3.79304328907968));
#18587=CARTESIAN_POINT('Ctrl Pts',(7.49902488252034,0.469014012275352,3.7886269543448));
#18588=CARTESIAN_POINT('Ctrl Pts',(7.51528614811584,0.385622987645243,3.78421969235287));
#18589=CARTESIAN_POINT('Ctrl Pts',(7.5272247353734,0.301290779278597,3.77981243036094));
#18590=CARTESIAN_POINT('Ctrl Pts',(7.53474649504538,0.216478700117246,3.77540516836901));
#18591=CARTESIAN_POINT('Ctrl Pts',(7.54112669174311,0.144538386814042,3.77166678803871));
#18592=CARTESIAN_POINT('Ctrl Pts',(7.54432979256689,0.0722532055568052,
3.76792840770841));
#18593=CARTESIAN_POINT('Ctrl Pts',(7.54432715382295,-8.9383613589154E-5,
3.76419002737811));
#18594=CARTESIAN_POINT('',(7.5454861976999,-0.00208864731307865,2.96419002737811));
#18595=CARTESIAN_POINT('Ctrl Pts',(7.54033673373089,-9.04938769800744E-5,
3.7641899623766));
#18596=CARTESIAN_POINT('Ctrl Pts',(7.54046778980184,-0.402997665835575,
3.74333534561196));
#18597=CARTESIAN_POINT('Ctrl Pts',(7.25582894391592,-1.62248956602737,3.68020497101128));
#18598=CARTESIAN_POINT('Ctrl Pts',(5.3347574418693,-2.88488257368372,3.57479883857445));
#18599=CARTESIAN_POINT('Ctrl Pts',(2.80334608662769,-1.77039299032977,3.44797156506626));
#18600=CARTESIAN_POINT('Ctrl Pts',(2.36277426232799,0.960179650799704,3.32114429155803));
#18601=CARTESIAN_POINT('Ctrl Pts',(4.41521293602296,2.81426324426903,3.19431701804983));
#18602=CARTESIAN_POINT('Ctrl Pts',(6.92189643281657,2.14358447382013,3.07533226332317));
#18603=CARTESIAN_POINT('Ctrl Pts',(7.53950298244955,0.659618068710635,2.99862326643261));
#18604=CARTESIAN_POINT('Ctrl Pts',(7.5454861976999,-0.00208864731307865,
2.96419002737811));
#18605=CARTESIAN_POINT('',(7.54690838528974,0.00161708353963758,2.16419002737811));
#18606=CARTESIAN_POINT('Ctrl Pts',(7.5454861976999,-0.00208864731307865,
2.96419002737811));
#18607=CARTESIAN_POINT('Ctrl Pts',(7.5468489355446,-0.152799050714208,2.95634750859654));
#18608=CARTESIAN_POINT('Ctrl Pts',(7.46563606218028,-1.11446191626834,2.90622923197887));
#18609=CARTESIAN_POINT('Ctrl Pts',(6.19420942661396,-2.67763958070757,2.81383519752519));
#18610=CARTESIAN_POINT('Ctrl Pts',(3.4444784365408,-2.3791266612517,2.68700792401695));
#18611=CARTESIAN_POINT('Ctrl Pts',(2.2003366210504,0.0911449075841722,2.56018065050874));
#18612=CARTESIAN_POINT('Ctrl Pts',(3.59748465251696,2.47821588663366,2.43335337700052));
#18613=CARTESIAN_POINT('Ctrl Pts',(6.36055187866693,2.6030757465843,2.30652610349231));
#18614=CARTESIAN_POINT('Ctrl Pts',(7.49721262842552,1.01042402016213,2.2168049869515));
#18615=CARTESIAN_POINT('Ctrl Pts',(7.54766542960058,0.100812120060077,2.16935962824677));
#18616=CARTESIAN_POINT('Ctrl Pts',(7.54690838528974,0.00161708353963758,
2.16419002737811));
#18617=CARTESIAN_POINT('',(7.54409003691263,0.000907487678406939,1.36419006975599));
#18618=CARTESIAN_POINT('Ctrl Pts',(7.54690838528974,0.00161708353963758,
2.16419002737811));
#18619=CARTESIAN_POINT('Ctrl Pts',(7.54147450253107,-0.710381132382711,
2.1270838704107));
#18620=CARTESIAN_POINT('Ctrl Pts',(6.84050801399482,-2.24289646830409,2.0477019556072));
#18621=CARTESIAN_POINT('Ctrl Pts',(4.2394355612513,-2.76597358458354,1.92604428296767));
#18622=CARTESIAN_POINT('Ctrl Pts',(2.30775733339397,-0.786390369643382,
1.79921700945943));
#18623=CARTESIAN_POINT('Ctrl Pts',(2.91931117988549,1.91104032894591,1.67238973595123));
#18624=CARTESIAN_POINT('Ctrl Pts',(5.51584714400404,2.86399965016062,1.545562462443));
#18625=CARTESIAN_POINT('Ctrl Pts',(7.30705101622796,1.51821913659295,1.4428294452149));
#18626=CARTESIAN_POINT('Ctrl Pts',(7.54182191684067,0.352067414377056,1.38237218582286));
#18627=CARTESIAN_POINT('Ctrl Pts',(7.54065407381936,0.00091808464348145,
1.3641906842669));
#18628=CARTESIAN_POINT('',(7.5443261628818,-0.00220558177832077,0.564190027336024));
#18629=CARTESIAN_POINT('Ctrl Pts',(7.54432698768978,0.000906756890839775,
1.36419002737811));
#18630=CARTESIAN_POINT('Ctrl Pts',(7.54435782807604,-0.0824390242491621,
1.35988108514997));
#18631=CARTESIAN_POINT('Ctrl Pts',(7.54013222037994,-0.165757790068172,
1.35557214292182));
#18632=CARTESIAN_POINT('Ctrl Pts',(7.53168467216415,-0.24859802536523,1.35126320069368));
#18633=CARTESIAN_POINT('Ctrl Pts',(7.52323186801572,-0.33148980256364,1.34695157750894));
#18634=CARTESIAN_POINT('Ctrl Pts',(7.5105519419166,-0.413902023721914,1.34263995432421));
#18635=CARTESIAN_POINT('Ctrl Pts',(7.49373099221603,-0.495390577514945,
1.33832833113947));
#18636=CARTESIAN_POINT('Ctrl Pts',(7.47688164180653,-0.577016717635693,
1.3340094281544));
#18637=CARTESIAN_POINT('Ctrl Pts',(7.45587739507288,-0.657715648835246,
1.32969052516934));
#18638=CARTESIAN_POINT('Ctrl Pts',(7.43085500839889,-0.7370556726297,1.32537162218427));
#18639=CARTESIAN_POINT('Ctrl Pts',(7.40580967646491,-0.816468450374359,
1.32104875881153));
#18640=CARTESIAN_POINT('Ctrl Pts',(7.37673901636463,-0.894519430353402,
1.31672589543878));
#18641=CARTESIAN_POINT('Ctrl Pts',(7.34382811427781,-0.970796546804707,
1.31240303206603));
#18642=CARTESIAN_POINT('Ctrl Pts',(7.31084909359606,-1.04723154072724,1.30807122128194));
#18643=CARTESIAN_POINT('Ctrl Pts',(7.27401414562565,-1.12188494603021,1.30373941049784));
#18644=CARTESIAN_POINT('Ctrl Pts',(7.23355454876966,-1.19436884264902,1.29940759971374));
#18645=CARTESIAN_POINT('Ctrl Pts',(7.21020525229532,-1.23619941248372,1.29690770495135));
#18646=CARTESIAN_POINT('Ctrl Pts',(7.18564959734902,-1.27730796117003,1.29440781018896));
#18647=CARTESIAN_POINT('Ctrl Pts',(7.15993834715027,-1.3176246785575,1.29190791542657));
#18648=CARTESIAN_POINT('Ctrl Pts',(7.11641158845541,-1.38587713674324,1.28767582576761));
#18649=CARTESIAN_POINT('Ctrl Pts',(7.06941799814008,-1.45209778396878,1.28344373610865));
#18650=CARTESIAN_POINT('Ctrl Pts',(7.01917337655043,-1.5159129852687,1.27921164644969));
#18651=CARTESIAN_POINT('Ctrl Pts',(6.96900056652542,-1.57963697940439,1.27498560545764));
#18652=CARTESIAN_POINT('Ctrl Pts',(6.91558623874066,-1.64096199371701,1.27075956446559));
#18653=CARTESIAN_POINT('Ctrl Pts',(6.85919010319566,-1.69954226565206,1.26653352347354));
#18654=CARTESIAN_POINT('Ctrl Pts',(6.80277845544641,-1.7581386505554,1.26230632007541));
#18655=CARTESIAN_POINT('Ctrl Pts',(6.74338363238152,-1.81398840427747,1.25807911667728));
#18656=CARTESIAN_POINT('Ctrl Pts',(6.68130671328084,-1.8667776791785,1.25385191327915));
#18657=CARTESIAN_POINT('Ctrl Pts',(6.61935791371015,-1.91945800316529,1.24963343433642));
#18658=CARTESIAN_POINT('Ctrl Pts',(6.55473841593925,-1.96909014855919,1.2454149553937));
#18659=CARTESIAN_POINT('Ctrl Pts',(6.48778380992533,-2.01539948780698,1.24119647645097));
#18660=CARTESIAN_POINT('Ctrl Pts',(6.42085115986977,-2.06169364115517,1.23697938084471));
#18661=CARTESIAN_POINT('Ctrl Pts',(6.35158530413795,-2.10466688812074,1.23276228523846));
#18662=CARTESIAN_POINT('Ctrl Pts',(6.2803525799754,-2.14408667431198,1.2285451896322));
#18663=CARTESIAN_POINT('Ctrl Pts',(6.20912141897576,-2.18350559545771,1.22432818656778));
#18664=CARTESIAN_POINT('Ctrl Pts',(6.13592388250251,-2.21937098687598,1.22011118350336));
#18665=CARTESIAN_POINT('Ctrl Pts',(6.06115152472861,-2.25149590597135,1.21589418043894));
#18666=CARTESIAN_POINT('Ctrl Pts',(5.98606960786372,-2.28375382288903,1.21165971889556));
#18667=CARTESIAN_POINT('Ctrl Pts',(5.90940023074154,-2.312240032171,1.20742525735218));
#18668=CARTESIAN_POINT('Ctrl Pts',(5.83155902235847,-2.33681448612258,1.2031907958088));
#18669=CARTESIAN_POINT('Ctrl Pts',(5.7539263582488,-2.36132310268867,1.19896767880546));
#18670=CARTESIAN_POINT('Ctrl Pts',(5.67512859653247,-2.38194081858851,1.19474456180213));
#18671=CARTESIAN_POINT('Ctrl Pts',(5.59559036205877,-2.39857956601335,1.19052144479879));
#18672=CARTESIAN_POINT('Ctrl Pts',(5.51573163278742,-2.41528535832578,1.18628131098539));
#18673=CARTESIAN_POINT('Ctrl Pts',(5.43512691782418,-2.42797998358737,1.18204117717198));
#18674=CARTESIAN_POINT('Ctrl Pts',(5.3542114637486,-2.4366268204207,1.17780104335858));
#18675=CARTESIAN_POINT('Ctrl Pts',(5.27329600967303,-2.44527365725402,1.17356090954517));
#18676=CARTESIAN_POINT('Ctrl Pts',(5.1920702865861,-2.44987274134868,1.16932077573176));
#18677=CARTESIAN_POINT('Ctrl Pts',(5.11096794520243,-2.45044005095549,1.16508064191836));
#18678=CARTESIAN_POINT('Ctrl Pts',(5.03001946683071,-2.45100628429295,1.16084855225939));
#18679=CARTESIAN_POINT('Ctrl Pts',(4.94889190026816,-2.44755815532954,1.15661646260043));
#18680=CARTESIAN_POINT('Ctrl Pts',(4.8680161635081,-2.44007369682082,1.15238437294146));
#18681=CARTESIAN_POINT('Ctrl Pts',(4.78725601749221,-2.43259993539089,1.14815833194941));
#18682=CARTESIAN_POINT('Ctrl Pts',(4.70674744527386,-2.4211013444984,1.14393229095736));
#18683=CARTESIAN_POINT('Ctrl Pts',(4.62692183838578,-2.40560796367452,1.13970624996531));
#18684=CARTESIAN_POINT('Ctrl Pts',(4.54707427483165,-2.3901103212734,1.13547904656717));
#18685=CARTESIAN_POINT('Ctrl Pts',(4.46791051861151,-2.37061571435661,1.13125184316904));
#18686=CARTESIAN_POINT('Ctrl Pts',(4.38985766079624,-2.34720625437829,1.12702463977091));
#18687=CARTESIAN_POINT('Ctrl Pts',(4.31196589498755,-2.32384510879852,1.12280616082819));
#18688=CARTESIAN_POINT('Ctrl Pts',(4.23518089894569,-2.29658536317591,1.11858768188546));
#18689=CARTESIAN_POINT('Ctrl Pts',(4.15991560342905,-2.26555941502226,1.11436920294274));
#18690=CARTESIAN_POINT('Ctrl Pts',(4.08467498913727,-2.23454364099199,1.11015210733648));
#18691=CARTESIAN_POINT('Ctrl Pts',(4.01095351498968,-2.199764294038,1.10593501173021));
#18692=CARTESIAN_POINT('Ctrl Pts',(3.93914551097837,-2.16140244977957,1.10171791612395));
#18693=CARTESIAN_POINT('Ctrl Pts',(3.86733908275442,-2.12304144735082,1.09750091305954));
#18694=CARTESIAN_POINT('Ctrl Pts',(3.79744645050496,-2.08109832390305,1.09328390999513));
#18695=CARTESIAN_POINT('Ctrl Pts',(3.72983736708083,-2.03580011475001,1.08906690693073));
#18696=CARTESIAN_POINT('Ctrl Pts',(3.66194838066793,-1.9903143700842,1.08483244538734));
#18697=CARTESIAN_POINT('Ctrl Pts',(3.59636229036309,-1.9414459522043,1.08059798384396));
#18698=CARTESIAN_POINT('Ctrl Pts',(3.53342257406746,-1.88946759495649,1.07636352230058));
#18699=CARTESIAN_POINT('Ctrl Pts',(3.47065147947842,-1.83762849285346,1.07214040529724));
#18700=CARTESIAN_POINT('Ctrl Pts',(3.41051291467663,-1.78269643951463,1.0679172882939));
#18701=CARTESIAN_POINT('Ctrl Pts',(3.35331161785885,-1.72497997478028,1.06369417129057));
#18702=CARTESIAN_POINT('Ctrl Pts',(3.29587983166491,-1.6670309448299,1.05945403747716));
#18703=CARTESIAN_POINT('Ctrl Pts',(3.24140934282728,-1.6062753736399,1.05521390366376));
#18704=CARTESIAN_POINT('Ctrl Pts',(3.19016748139266,-1.54305868176037,1.05097376985035));
#18705=CARTESIAN_POINT('Ctrl Pts',(3.13892561995805,-1.47984198988085,1.04673363603695));
#18706=CARTESIAN_POINT('Ctrl Pts',(3.09091261150796,-1.41416459129448,1.04249350222354));
#18707=CARTESIAN_POINT('Ctrl Pts',(3.04635076874628,-1.34639915919387,1.03825336841014));
#18708=CARTESIAN_POINT('Ctrl Pts',(3.00187346632254,-1.27876228803632,1.03402127875118));
#18709=CARTESIAN_POINT('Ctrl Pts',(2.96066829775093,-1.20879296809767,1.02978918909222));
#18710=CARTESIAN_POINT('Ctrl Pts',(2.9229879400944,-1.1368409524031,1.02555709943326));
#18711=CARTESIAN_POINT('Ctrl Pts',(2.88536143666856,-1.06499177332402,1.02133105844122));
#18712=CARTESIAN_POINT('Ctrl Pts',(2.85124995232455,-0.991165934832547,
1.01710501744917));
#18713=CARTESIAN_POINT('Ctrl Pts',(2.82086276928575,-0.915741857301956,
1.01287897645713));
#18714=CARTESIAN_POINT('Ctrl Pts',(2.79046722801125,-0.840297033780658,
1.008651773059));
#18715=CARTESIAN_POINT('Ctrl Pts',(2.76379827099131,-0.763253495899821,
1.00442456966086));
#18716=CARTESIAN_POINT('Ctrl Pts',(2.74101913587287,-0.685014359702723,
1.00019736626273));
#18717=CARTESIAN_POINT('Ctrl Pts',(2.71828701423593,-0.606936699969137,
0.995978887320007));
#18718=CARTESIAN_POINT('Ctrl Pts',(2.69942882816898,-0.527668811345698,
0.991760408377288));
#18719=CARTESIAN_POINT('Ctrl Pts',(2.68455791009646,-0.447629258849976,
0.987541929434567));
#18720=CARTESIAN_POINT('Ctrl Pts',(2.66969186854068,-0.367615953168051,
0.983324833828307));
#18721=CARTESIAN_POINT('Ctrl Pts',(2.65881058318793,-0.286831942657926,
0.979107738222049));
#18722=CARTESIAN_POINT('Ctrl Pts',(2.65197641713918,-0.205706640135218,
0.974890642615789));
#18723=CARTESIAN_POINT('Ctrl Pts',(2.64514240106244,-0.124583117862515,
0.970673639551366));
#18724=CARTESIAN_POINT('Ctrl Pts',(2.64235536557133,-0.0431187816132713,
0.966456636486941));
#18725=CARTESIAN_POINT('Ctrl Pts',(2.64362573752005,0.0382526019873604,
0.962239633422518));
#18726=CARTESIAN_POINT('Ctrl Pts',(2.64490136883462,0.119960864780826,0.958005171879135));
#18727=CARTESIAN_POINT('Ctrl Pts',(2.65026808016463,0.201574931687601,0.953770710335755));
#18728=CARTESIAN_POINT('Ctrl Pts',(2.65968365842976,0.282658249302825,0.949536248792372));
#18729=CARTESIAN_POINT('Ctrl Pts',(2.66907401143222,0.363524336714318,0.945313131789035));
#18730=CARTESIAN_POINT('Ctrl Pts',(2.68249144681184,0.44386206065688,0.941090014785696));
#18731=CARTESIAN_POINT('Ctrl Pts',(2.6998426393241,0.5232479207169,0.93686689778236));
#18732=CARTESIAN_POINT('Ctrl Pts',(2.71726374748095,0.602953661590489,0.932626763968954));
#18733=CARTESIAN_POINT('Ctrl Pts',(2.73865024951101,0.681699398718007,0.928386630155549));
#18734=CARTESIAN_POINT('Ctrl Pts',(2.76385752974272,0.759072982832998,0.924146496342143));
#18735=CARTESIAN_POINT('Ctrl Pts',(2.78906480997443,0.836446566947988,0.919906362528737));
#18736=CARTESIAN_POINT('Ctrl Pts',(2.81809264355031,0.912447583674052,0.91566622871533));
#18737=CARTESIAN_POINT('Ctrl Pts',(2.85074906954626,0.986686855352023,0.911426094901924));
#18738=CARTESIAN_POINT('Ctrl Pts',(2.8833435415224,1.06078528426571,0.907194005242962));
#18739=CARTESIAN_POINT('Ctrl Pts',(2.91967443931081,1.13340509916211,0.902961915583999));
#18740=CARTESIAN_POINT('Ctrl Pts',(2.95958554566783,1.20414409480807,0.898729825925037));
#18741=CARTESIAN_POINT('Ctrl Pts',(2.99943960952148,1.27478198753391,0.894503784932993));
#18742=CARTESIAN_POINT('Ctrl Pts',(3.04286349264554,1.34354399861238,0.890277743940949));
#18743=CARTESIAN_POINT('Ctrl Pts',(3.08965332706236,1.41004876355166,0.886051702948905));
#18744=CARTESIAN_POINT('Ctrl Pts',(3.13645603139418,1.47657182115393,0.881824499550772));
#18745=CARTESIAN_POINT('Ctrl Pts',(3.18662632694945,1.54083597478271,0.87759729615264));
#18746=CARTESIAN_POINT('Ctrl Pts',(3.23991458832617,1.60248508368995,0.873370092754507));
#18747=CARTESIAN_POINT('Ctrl Pts',(3.29309286893867,1.66400695601759,0.869151613811782));
#18748=CARTESIAN_POINT('Ctrl Pts',(3.34937597300426,1.72292419920925,0.864933134869057));
#18749=CARTESIAN_POINT('Ctrl Pts',(3.4084741804018,1.77891416304601,0.860714655926333));
#18750=CARTESIAN_POINT('Ctrl Pts',(3.46755300813528,1.8348857664834,0.856497560320065));
#18751=CARTESIAN_POINT('Ctrl Pts',(3.52944476885911,1.88793167753747,0.852280464713795));
#18752=CARTESIAN_POINT('Ctrl Pts',(3.59382293133738,1.93776613078952,0.848063369107527));
#18753=CARTESIAN_POINT('Ctrl Pts',(3.65819968107221,1.98759949045183,0.843846366043108));
#18754=CARTESIAN_POINT('Ctrl Pts',(3.72506235591399,2.03422124889516,0.839629362978691));
#18755=CARTESIAN_POINT('Ctrl Pts',(3.79405253868528,2.07738686710156,0.835412359914272));
#18756=CARTESIAN_POINT('Ctrl Pts',(3.86332834222469,2.12073119185045,0.831177898370891));
#18757=CARTESIAN_POINT('Ctrl Pts',(3.93474891393538,2.16059043725314,0.82694343682751));
#18758=CARTESIAN_POINT('Ctrl Pts',(4.00792488348466,2.19676273314479,0.822708975284129));
#18759=CARTESIAN_POINT('Ctrl Pts',(4.08090480739543,2.23283811988869,0.818485858280795));
#18760=CARTESIAN_POINT('Ctrl Pts',(4.15563029003622,2.26524613902794,0.814262741277461));
#18761=CARTESIAN_POINT('Ctrl Pts',(4.23169513360672,2.29383491709998,0.810039624274127));
#18762=CARTESIAN_POINT('Ctrl Pts',(4.30806647614351,2.32253889202927,0.805799490460723));
#18763=CARTESIAN_POINT('Ctrl Pts',(4.38578754448091,2.34739264670183,0.801559356647321));
#18764=CARTESIAN_POINT('Ctrl Pts',(4.46443378799616,2.368293528894,0.797319222833917));
#18765=CARTESIAN_POINT('Ctrl Pts',(4.54308003151142,2.38919441108618,0.793079089020514));
#18766=CARTESIAN_POINT('Ctrl Pts',(4.62265098016665,2.40614238428662,0.788838955207109));
#18767=CARTESIAN_POINT('Ctrl Pts',(4.7027156287509,2.41908702275893,0.784598821393705));
#18768=CARTESIAN_POINT('Ctrl Pts',(4.78262838297833,2.43200710335745,0.780366731734741));
#18769=CARTESIAN_POINT('Ctrl Pts',(4.86333110127275,2.44098724308894,0.776134642075777));
#18770=CARTESIAN_POINT('Ctrl Pts',(4.94440127321378,2.44593993297403,0.771902552416813));
#18771=CARTESIAN_POINT('Ctrl Pts',(5.02535557651595,2.45088554428235,0.767676511424783));
#18772=CARTESIAN_POINT('Ctrl Pts',(5.10667583045401,2.45181511005929,0.763450470432753));
#18773=CARTESIAN_POINT('Ctrl Pts',(5.18793111540846,2.44869244592307,0.759224429440723));
#18774=CARTESIAN_POINT('Ctrl Pts',(5.26920875027372,2.44556892287331,0.754997226042588));
#18775=CARTESIAN_POINT('Ctrl Pts',(5.35042091607538,2.43839089225648,0.750770022644452));
#18776=CARTESIAN_POINT('Ctrl Pts',(5.43113299206482,2.42717428764143,0.746542819246317));
#18777=CARTESIAN_POINT('Ctrl Pts',(5.51167848773102,2.41598083279176,0.742324340303598));
#18778=CARTESIAN_POINT('Ctrl Pts',(5.59172549204092,2.40076549679287,0.73810586136088));
#18779=CARTESIAN_POINT('Ctrl Pts',(5.67084570003744,2.38159607179844,0.73388738241816));
#18780=CARTESIAN_POINT('Ctrl Pts',(5.74993996269457,2.3624329329002,0.729670286811894));
#18781=CARTESIAN_POINT('Ctrl Pts',(5.82810758131809,2.33931838934476,0.725453191205628));
#18782=CARTESIAN_POINT('Ctrl Pts',(5.90493120065128,2.31237118081487,0.721236095599362));
#18783=CARTESIAN_POINT('Ctrl Pts',(5.98175313413231,2.28542456362669,0.717019092534944));
#18784=CARTESIAN_POINT('Ctrl Pts',(6.05723068884862,2.25464560358275,0.712802089470526));
#18785=CARTESIAN_POINT('Ctrl Pts',(6.13096378062545,2.22020221392695,0.708585086406108));
#18786=CARTESIAN_POINT('Ctrl Pts',(6.20500212891083,2.18561622793326,0.704350624862723));
#18787=CARTESIAN_POINT('Ctrl Pts',(6.27728110634971,2.14733559408323,0.700116163319338));
#18788=CARTESIAN_POINT('Ctrl Pts',(6.34741961762619,2.10557740033057,0.695881701775953));
#18789=CARTESIAN_POINT('Ctrl Pts',(6.4173702209143,2.06393108089692,0.69165858477262));
#18790=CARTESIAN_POINT('Ctrl Pts',(6.48519144589893,2.0188261044308,0.687435467769287));
#18791=CARTESIAN_POINT('Ctrl Pts',(6.55053501525511,1.97052086037958,0.683212350765954));
#18792=CARTESIAN_POINT('Ctrl Pts',(6.61614188281229,1.92202097309134,0.678972216952543));
#18793=CARTESIAN_POINT('Ctrl Pts',(6.679250726288,1.87029527870244,0.674732083139132));
#18794=CARTESIAN_POINT('Ctrl Pts',(6.73954460630417,1.8156443269441,0.67049194932572));
#18795=CARTESIAN_POINT('Ctrl Pts',(6.79983848632033,1.76099337518576,0.666251815512309));
#18796=CARTESIAN_POINT('Ctrl Pts',(6.85731711672739,1.70341754074066,0.662011681698898));
#18797=CARTESIAN_POINT('Ctrl Pts',(6.91170388622064,1.64325118035374,0.657771547885487));
#18798=CARTESIAN_POINT('Ctrl Pts',(6.96540918855505,1.58383870549914,0.653584543021816));
#18799=CARTESIAN_POINT('Ctrl Pts',(7.01630972610991,1.52166769401119,0.649397538158145));
#18800=CARTESIAN_POINT('Ctrl Pts',(7.06410492824259,1.45703663236438,0.645210533294474));
#18801=CARTESIAN_POINT('Ctrl Pts',(7.11183727288974,1.3924905697518,0.641029034937438));
#18802=CARTESIAN_POINT('Ctrl Pts',(7.15647210340004,1.32549125271794,0.636847536580401));
#18803=CARTESIAN_POINT('Ctrl Pts',(7.19774685860031,1.25637260902529,0.632666038223364));
#18804=CARTESIAN_POINT('Ctrl Pts',(7.23898061525822,1.18732262143072,0.628488693381877));
#18805=CARTESIAN_POINT('Ctrl Pts',(7.27686067727665,1.11615789015537,0.62431134854039));
#18806=CARTESIAN_POINT('Ctrl Pts',(7.31116678822456,1.04324263857501,0.620134003698903));
#18807=CARTESIAN_POINT('Ctrl Pts',(7.34544985857217,0.970376358187296,0.615959464437243));
#18808=CARTESIAN_POINT('Ctrl Pts',(7.37616354180696,0.895762320608089,0.611784925175584));
#18809=CARTESIAN_POINT('Ctrl Pts',(7.40313346543961,0.819789373349364,0.607610385913924));
#18810=CARTESIAN_POINT('Ctrl Pts',(7.43010088435227,0.743823481763554,0.603436234345314));
#18811=CARTESIAN_POINT('Ctrl Pts',(7.45332506264281,0.666499374329233,0.599262082776703));
#18812=CARTESIAN_POINT('Ctrl Pts',(7.47268021978743,0.588224743025335,0.595087931208093));
#18813=CARTESIAN_POINT('Ctrl Pts',(7.49203419135605,0.509954906336266,0.590914035321927));
#18814=CARTESIAN_POINT('Ctrl Pts',(7.50751950632686,0.430735124923251,0.58674013943576));
#18815=CARTESIAN_POINT('Ctrl Pts',(7.51906109382869,0.350985176540635,0.582566243549594));
#18816=CARTESIAN_POINT('Ctrl Pts',(7.53061059387695,0.271180554122189,0.578389486172757));
#18817=CARTESIAN_POINT('Ctrl Pts',(7.5382109109335,0.190845511248738,0.574212728795923));
#18818=CARTESIAN_POINT('Ctrl Pts',(7.54183875718163,0.110405832285044,0.570035971419086));
#18819=CARTESIAN_POINT('Ctrl Pts',(7.54353131309223,0.0728770494303689,
0.568087323405428));
#18820=CARTESIAN_POINT('Ctrl Pts',(7.54435994289275,0.0353255197735597,
0.566138675391768));
#18821=CARTESIAN_POINT('Ctrl Pts',(7.54432616288253,-0.00220558096774611,
0.56419002737811));
#18822=CARTESIAN_POINT('',(7.54432706310264,0.000672762683496843,-0.235809972659579));
#18823=CARTESIAN_POINT('Ctrl Pts',(7.5443261628818,-0.00220558177831103,
0.564190027336024));
#18824=CARTESIAN_POINT('Ctrl Pts',(7.54423010976538,-0.108924846857774,
0.558649068509566));
#18825=CARTESIAN_POINT('Ctrl Pts',(7.53715829815171,-0.215335078947692,
0.553108109683107));
#18826=CARTESIAN_POINT('Ctrl Pts',(7.52325695306015,-0.320657306947822,
0.547567150856648));
#18827=CARTESIAN_POINT('Ctrl Pts',(7.50935560796858,-0.425979534947946,
0.542026192030189));
#18828=CARTESIAN_POINT('Ctrl Pts',(7.48862491996705,-0.530214102573748,
0.53648523320373));
#18829=CARTESIAN_POINT('Ctrl Pts',(7.46126409479691,-0.632607768076282,
0.530944274377271));
#18830=CARTESIAN_POINT('Ctrl Pts',(7.4403663641171,-0.710814299921907,0.526712184718308));
#18831=CARTESIAN_POINT('Ctrl Pts',(7.4155502457108,-0.788130093372859,0.522480095059343));
#18832=CARTESIAN_POINT('Ctrl Pts',(7.38690870987743,-0.864133806050284,
0.518248005400379));
#18833=CARTESIAN_POINT('Ctrl Pts',(7.35830810963951,-0.940028891269548,
0.514021964408331));
#18834=CARTESIAN_POINT('Ctrl Pts',(7.32589311339092,-1.0146151890148,0.509795923416282));
#18835=CARTESIAN_POINT('Ctrl Pts',(7.28980696566903,-1.08748467719048,0.505569882424235));
#18836=CARTESIAN_POINT('Ctrl Pts',(7.25371089216605,-1.16037420869669,0.501342679026102));
#18837=CARTESIAN_POINT('Ctrl Pts',(7.21394179334593,-1.23154554265047,0.497115475627969));
#18838=CARTESIAN_POINT('Ctrl Pts',(7.17069198614245,-1.30060859794395,0.492888272229837));
#18839=CARTESIAN_POINT('Ctrl Pts',(7.12753144150309,-1.36952911513612,0.488669793287112));
#18840=CARTESIAN_POINT('Ctrl Pts',(7.08090476714694,-1.43634964032899,0.484451314344387));
#18841=CARTESIAN_POINT('Ctrl Pts',(7.03104901840703,-1.5007070679161,0.480232835401663));
#18842=CARTESIAN_POINT('Ctrl Pts',(6.98120961851607,-1.56504339121959,0.476015739795398));
#18843=CARTESIAN_POINT('Ctrl Pts',(6.92814353145569,-1.626917853877,0.471798644189134));
#18844=CARTESIAN_POINT('Ctrl Pts',(6.87212982415058,-1.68599818164299,0.46758154858287));
#18845=CARTESIAN_POINT('Ctrl Pts',(6.81611734603551,-1.74507721292363,0.463364545518452));
#18846=CARTESIAN_POINT('Ctrl Pts',(6.75715769683451,-1.80136189479566,0.459147542454036));
#18847=CARTESIAN_POINT('Ctrl Pts',(6.69556775059078,-1.85455582711549,0.454930539389618));
#18848=CARTESIAN_POINT('Ctrl Pts',(6.63372282070953,-1.90796998340342,0.450696077846238));
#18849=CARTESIAN_POINT('Ctrl Pts',(6.56922611707182,-1.95826742595693,0.446461616302857));
#18850=CARTESIAN_POINT('Ctrl Pts',(6.50243161924799,-2.00518919670368,0.442227154759477));
#18851=CARTESIAN_POINT('Ctrl Pts',(6.43581607047058,-2.05198525939953,0.438004037756142));
#18852=CARTESIAN_POINT('Ctrl Pts',(6.36691544130841,-2.09542350017295,0.433780920752806));
#18853=CARTESIAN_POINT('Ctrl Pts',(6.29610797575104,-2.13529180187246,0.429557803749471));
#18854=CARTESIAN_POINT('Ctrl Pts',(6.22501519553347,-2.17532075062892,0.425317669936068));
#18855=CARTESIAN_POINT('Ctrl Pts',(6.152000605206,-2.21175072707879,0.421077536122665));
#18856=CARTESIAN_POINT('Ctrl Pts',(6.07746810223484,-2.24441545570653,0.416837402309262));
#18857=CARTESIAN_POINT('Ctrl Pts',(6.0029355992637,-2.27708018433426,0.41259726849586));
#18858=CARTESIAN_POINT('Ctrl Pts',(5.9268856425996,-2.30597955728391,0.408357134682459));
#18859=CARTESIAN_POINT('Ctrl Pts',(5.84973648336748,-2.33099792749201,0.404117000869056));
#18860=CARTESIAN_POINT('Ctrl Pts',(5.77273368738216,-2.35596883419008,0.399884911210094));
#18861=CARTESIAN_POINT('Ctrl Pts',(5.69434857887907,-2.3771666268737,0.395652821551131));
#18862=CARTESIAN_POINT('Ctrl Pts',(5.61498535135581,-2.39444030722076,0.391420731892169));
#18863=CARTESIAN_POINT('Ctrl Pts',(5.53573555283973,-2.41168929935297,0.387194690900119));
#18864=CARTESIAN_POINT('Ctrl Pts',(5.45551086207904,-2.42502522022467,0.38296864990807));
#18865=CARTESIAN_POINT('Ctrl Pts',(5.37473162020496,-2.43434651019169,0.37874260891602));
#18866=CARTESIAN_POINT('Ctrl Pts',(5.29393015935994,-2.44367036405342,0.374515405517887));
#18867=CARTESIAN_POINT('Ctrl Pts',(5.21257429382919,-2.448977259706,0.370288202119756));
#18868=CARTESIAN_POINT('Ctrl Pts',(5.1310959806596,-2.45021657913494,0.366060998721624));
#18869=CARTESIAN_POINT('Ctrl Pts',(5.04978582923741,-2.45145334075294,0.3618425197789));
#18870=CARTESIAN_POINT('Ctrl Pts',(4.968354199392,-2.4486392673208,0.357624040836176));
#18871=CARTESIAN_POINT('Ctrl Pts',(4.88723472502712,-2.44177595567052,0.353405561893452));
#18872=CARTESIAN_POINT('Ctrl Pts',(4.80614185160729,-2.4349148946583,0.349188466287189));
#18873=CARTESIAN_POINT('Ctrl Pts',(4.72536139306099,-2.4240072715402,0.344971370680927));
#18874=CARTESIAN_POINT('Ctrl Pts',(4.64532394146638,-2.40910670520083,0.340754275074664));
#18875=CARTESIAN_POINT('Ctrl Pts',(4.56528824624972,-2.3942064658462,0.336537272010249));
#18876=CARTESIAN_POINT('Ctrl Pts',(4.48599598219529,-2.37531354366744,0.332320268945834));
#18877=CARTESIAN_POINT('Ctrl Pts',(4.40786818142602,-2.35253279168468,0.32810326588142));
#18878=CARTESIAN_POINT('Ctrl Pts',(4.32941692996307,-2.32965772692261,0.323868804338038));
#18879=CARTESIAN_POINT('Ctrl Pts',(4.25214026067396,-2.30286269210011,0.319634342794656));
#18880=CARTESIAN_POINT('Ctrl Pts',(4.17644794826881,-2.27230403780522,0.315399881251274));
#18881=CARTESIAN_POINT('Ctrl Pts',(4.10095842303284,-2.24182725315866,0.311176764247939));
#18882=CARTESIAN_POINT('Ctrl Pts',(4.02704518323412,-2.20760722330935,0.306953647244604));
#18883=CARTESIAN_POINT('Ctrl Pts',(3.9550918770022,-2.16984612717385,0.30273053024127));
#18884=CARTESIAN_POINT('Ctrl Pts',(3.88284863901013,-2.13193287484648,0.298490396427865));
#18885=CARTESIAN_POINT('Ctrl Pts',(3.812581564407,-2.09045020603706,0.29425026261446));
#18886=CARTESIAN_POINT('Ctrl Pts',(3.74464976856326,-2.04564675071359,0.290010128801055));
#18887=CARTESIAN_POINT('Ctrl Pts',(3.67671797271953,-2.00084329539013,0.285769994987649));
#18888=CARTESIAN_POINT('Ctrl Pts',(3.6111217956416,-1.95271938014768,0.281529861174244));
#18889=CARTESIAN_POINT('Ctrl Pts',(3.54818565973068,-1.90156320344629,0.277289727360839));
#18890=CARTESIAN_POINT('Ctrl Pts',(3.48536892288111,-1.85050407749949,0.273057637701877));
#18891=CARTESIAN_POINT('Ctrl Pts',(3.42496777694521,-1.79623370603101,0.268825548042916));
#18892=CARTESIAN_POINT('Ctrl Pts',(3.36732867519252,-1.73900927187232,0.264593458383954));
#18893=CARTESIAN_POINT('Ctrl Pts',(3.30977195348276,-1.68186662509753,0.260367417391908));
#18894=CARTESIAN_POINT('Ctrl Pts',(3.25496976256562,-1.62177862576476,0.256141376399862));
#18895=CARTESIAN_POINT('Ctrl Pts',(3.20323583655671,-1.55904288424455,0.251915335407816));
#18896=CARTESIAN_POINT('Ctrl Pts',(3.1514876807212,-1.49628988676115,0.247688132009683));
#18897=CARTESIAN_POINT('Ctrl Pts',(3.10280982282825,-1.43088800491758,0.243460928611549));
#18898=CARTESIAN_POINT('Ctrl Pts',(3.05747955297212,-1.36317228987018,0.239233725213416));
#18899=CARTESIAN_POINT('Ctrl Pts',(3.0122428395127,-1.29559633217082,0.235015246270693));
#18900=CARTESIAN_POINT('Ctrl Pts',(2.97034018911734,-1.22571645496426,0.230796767327972));
#18901=CARTESIAN_POINT('Ctrl Pts',(2.93200597649514,-1.15389749987109,0.22657828838525));
#18902=CARTESIAN_POINT('Ctrl Pts',(2.89368433454466,-1.08210209586836,0.222361192778988));
#18903=CARTESIAN_POINT('Ctrl Pts',(2.85892902515504,-1.00836928638529,0.218144097172723));
#18904=CARTESIAN_POINT('Ctrl Pts',(2.82792910448838,-0.933089638048898,
0.213927001566462));
#18905=CARTESIAN_POINT('Ctrl Pts',(2.79692986409794,-0.85781164168302,0.209709998502045));
#18906=CARTESIAN_POINT('Ctrl Pts',(2.76968602445696,-0.780987304074721,
0.205492995437632));
#18907=CARTESIAN_POINT('Ctrl Pts',(2.74633844139471,-0.703027017523819,
0.201275992373215));
#18908=CARTESIAN_POINT('Ctrl Pts',(2.72289419886089,-0.624743973791531,
0.197041530829833));
#18909=CARTESIAN_POINT('Ctrl Pts',(2.7033786904847,-0.545316003652663,0.192807069286448));
#18910=CARTESIAN_POINT('Ctrl Pts',(2.68788342794357,-0.465172043503821,
0.188572607743065));
#18911=CARTESIAN_POINT('Ctrl Pts',(2.67242967873884,-0.385242796927489,
0.184349490739732));
#18912=CARTESIAN_POINT('Ctrl Pts',(2.66097468660251,-0.304601860576383,
0.180126373736401));
#18913=CARTESIAN_POINT('Ctrl Pts',(2.65355729498284,-0.223681152716059,
0.175903256733068));
#18914=CARTESIAN_POINT('Ctrl Pts',(2.64611001540497,-0.142434379460049,
0.17166312291966));
#18915=CARTESIAN_POINT('Ctrl Pts',(2.64273295449464,-0.0609060466888589,
0.167422989106253));
#18916=CARTESIAN_POINT('Ctrl Pts',(2.64341263115474,0.0204672691777126,
0.163182855292845));
#18917=CARTESIAN_POINT('Ctrl Pts',(2.64409230781484,0.101840585044284,0.158942721479438));
#18918=CARTESIAN_POINT('Ctrl Pts',(2.64882863273646,0.183058421088749,0.15470258766603));
#18919=CARTESIAN_POINT('Ctrl Pts',(2.65755605430675,0.263691812006178,0.150462453852623));
#18920=CARTESIAN_POINT('Ctrl Pts',(2.66626691868095,0.344172229579254,0.146230364193661));
#18921=CARTESIAN_POINT('Ctrl Pts',(2.67898623277376,0.424370675316747,0.141998274534699));
#18922=CARTESIAN_POINT('Ctrl Pts',(2.69568645370933,0.503856551649249,0.137766184875736));
#18923=CARTESIAN_POINT('Ctrl Pts',(2.7123628060405,0.583228823680029,0.13354014388369));
#18924=CARTESIAN_POINT('Ctrl Pts',(2.73300867017065,0.661890098062354,0.129314102891644));
#18925=CARTESIAN_POINT('Ctrl Pts',(2.75754478458903,0.739415264644778,0.125088061899598));
#18926=CARTESIAN_POINT('Ctrl Pts',(2.78208764786025,0.816961755139046,0.120860858501465));
#18927=CARTESIAN_POINT('Ctrl Pts',(2.81052282522853,0.893371052255047,0.116633655103332));
#18928=CARTESIAN_POINT('Ctrl Pts',(2.8427198187342,0.968228283293912,0.112406451705199));
#18929=CARTESIAN_POINT('Ctrl Pts',(2.87485036139572,1.04293101772762,0.108187972762477));
#18930=CARTESIAN_POINT('Ctrl Pts',(2.9107270471507,1.11608764946936,0.103969493819754));
#18931=CARTESIAN_POINT('Ctrl Pts',(2.95017104523237,1.18730313362396,0.0997510148770315));
#18932=CARTESIAN_POINT('Ctrl Pts',(2.98960210871808,1.25849526458015,0.0955339192707685));
#18933=CARTESIAN_POINT('Ctrl Pts',(3.03259793643195,1.32774710588591,0.0913168236645044));
#18934=CARTESIAN_POINT('Ctrl Pts',(3.07893347085776,1.39468766746458,0.0870997280582415));
#18935=CARTESIAN_POINT('Ctrl Pts',(3.12526798847574,1.46162676006941,0.0828827249938237));
#18936=CARTESIAN_POINT('Ctrl Pts',(3.1749418016699,1.52625429236095,0.078665721929407));
#18937=CARTESIAN_POINT('Ctrl Pts',(3.22768701133789,1.58822895469187,0.0744487188649892));
#18938=CARTESIAN_POINT('Ctrl Pts',(3.28065058725305,1.6504601933928,0.0702142573216073));
#18939=CARTESIAN_POINT('Ctrl Pts',(3.33671074912355,1.710016181829,0.0659797957782236));
#18940=CARTESIAN_POINT('Ctrl Pts',(3.39555721020267,1.76658694749482,0.0617453342348417));
#18941=CARTESIAN_POINT('Ctrl Pts',(3.45424601580953,1.8230061545008,0.0575222172315082));
#18942=CARTESIAN_POINT('Ctrl Pts',(3.51570583031406,1.87645583795634,0.0532991002281749));
#18943=CARTESIAN_POINT('Ctrl Pts',(3.57959523468432,1.92666861191147,0.0490759832248413));
#18944=CARTESIAN_POINT('Ctrl Pts',(3.64374207778028,1.97708371538693,0.0448358494114354));
#18945=CARTESIAN_POINT('Ctrl Pts',(3.71033774211444,2.0242355030172,0.0405957155980312));
#18946=CARTESIAN_POINT('Ctrl Pts',(3.77900845618789,2.06789797573829,0.0363555817846253));
#18947=CARTESIAN_POINT('Ctrl Pts',(3.84767917026135,2.11156044845939,0.0321154479712191));
#18948=CARTESIAN_POINT('Ctrl Pts',(3.91842449697453,2.15173342960033,0.0278753141578127));
#18949=CARTESIAN_POINT('Ctrl Pts',(3.99084874874298,2.18823876309949,0.0236351803444066));
#18950=CARTESIAN_POINT('Ctrl Pts',(4.06313560110558,2.22467484063797,0.019403090685444));
#18951=CARTESIAN_POINT('Ctrl Pts',(4.13736469436463,2.25759312375906,0.0151710010264822));
#18952=CARTESIAN_POINT('Ctrl Pts',(4.21315963169909,2.28678266623765,0.0109389113675196));
#18953=CARTESIAN_POINT('Ctrl Pts',(4.28884623996522,2.31593048988839,0.00671287037547256));
#18954=CARTESIAN_POINT('Ctrl Pts',(4.36609381744558,2.34135999178187,0.00248682938342509));
#18955=CARTESIAN_POINT('Ctrl Pts',(4.44450245996956,2.362906618941,-0.00173921160862189));
#18956=CARTESIAN_POINT('Ctrl Pts',(4.52293266941243,2.38445917267079,-0.0059664150067547));
#18957=CARTESIAN_POINT('Ctrl Pts',(4.60252415455784,2.4021265292946,-0.010193618404886));
#18958=CARTESIAN_POINT('Ctrl Pts',(4.68285775296697,2.41579270638442,-0.0144208218030188));
#18959=CARTESIAN_POINT('Ctrl Pts',(4.7630255521866,2.42943067807664,-0.018639300745742));
#18960=CARTESIAN_POINT('Ctrl Pts',(4.84393195051431,2.43908386709367,-0.0228577796884664));
#18961=CARTESIAN_POINT('Ctrl Pts',(4.92514815533413,2.44468763749459,-0.0270762586311895));
#18962=CARTESIAN_POINT('Ctrl Pts',(5.00633772748878,2.45028957029004,-0.031293354237453));
#18963=CARTESIAN_POINT('Ctrl Pts',(5.08783644115347,2.45184468959132,-0.0355104498437151));
#18964=CARTESIAN_POINT('Ctrl Pts',(5.16921056632157,2.44934023593412,-0.0397275454499786));
#18965=CARTESIAN_POINT('Ctrl Pts',(5.25058290577918,2.44683583723579,-0.0439445485143945));
#18966=CARTESIAN_POINT('Ctrl Pts',(5.33183019774275,2.44027205814737,-0.0481615515788123));
#18967=CARTESIAN_POINT('Ctrl Pts',(5.41252033681973,2.42968823229451,-0.0523785546432283));
#18968=CARTESIAN_POINT('Ctrl Pts',(5.4935445347234,2.41906058918607,-0.0566130161866101));
#18969=CARTESIAN_POINT('Ctrl Pts',(5.57400648719356,2.40437959084643,-0.0608474777299928));
#18970=CARTESIAN_POINT('Ctrl Pts',(5.65347735077864,2.38573718352883,-0.0650819392733748));
#18971=CARTESIAN_POINT('Ctrl Pts',(5.73273530408329,2.36714472105883,-0.0693050562767073));
#18972=CARTESIAN_POINT('Ctrl Pts',(5.81100703423365,2.344612217432,-0.0735281732800393));
#18973=CARTESIAN_POINT('Ctrl Pts',(5.88788252018853,2.31828089923005,-0.0777512902833717));
#18974=CARTESIAN_POINT('Ctrl Pts',(5.96506777154723,2.29184348047714,-0.0819914240967782));
#18975=CARTESIAN_POINT('Ctrl Pts',(6.04084506816538,2.26157675118435,-0.0862315579101823));
#18976=CARTESIAN_POINT('Ctrl Pts',(6.1148215411939,2.22767159031258,-0.0904716917235886));
#18977=CARTESIAN_POINT('Ctrl Pts',(6.18879801422243,2.19376642944081,-0.0947118255369952));
#18978=CARTESIAN_POINT('Ctrl Pts',(6.26097327777241,2.15622310783766,-0.0989519593504032));
#18979=CARTESIAN_POINT('Ctrl Pts',(6.33098270718824,2.11527690641461,-0.10319209316381));
#18980=CARTESIAN_POINT('Ctrl Pts',(6.40085931846967,2.07440838592866,-0.107424182822774));
#18981=CARTESIAN_POINT('Ctrl Pts',(6.46883900936567,2.02999742697265,-0.111656272481739));
#18982=CARTESIAN_POINT('Ctrl Pts',(6.53454011865696,1.98224529452245,-0.115888362140703));
#18983=CARTESIAN_POINT('Ctrl Pts',(6.60014732537095,1.93456141127468,-0.120114403132748));
#18984=CARTESIAN_POINT('Ctrl Pts',(6.66348204576312,1.88354610978608,-0.124340444124791));
#18985=CARTESIAN_POINT('Ctrl Pts',(6.72418878096599,1.82944560456303,-0.128566485116836));
#18986=CARTESIAN_POINT('Ctrl Pts',(6.7849122140378,1.77533021856699,-0.132793688514969));
#18987=CARTESIAN_POINT('Ctrl Pts',(6.84300582713177,1.71812818962209,-0.137020891913102));
#18988=CARTESIAN_POINT('Ctrl Pts',(6.89814442098349,1.65812829880832,-0.141248095311235));
#18989=CARTESIAN_POINT('Ctrl Pts',(6.95316921520028,1.59825224078014,-0.145466574253956));
#18990=CARTESIAN_POINT('Ctrl Pts',(7.00525084276438,1.53559018352991,-0.149685053196679));
#18991=CARTESIAN_POINT('Ctrl Pts',(7.05410196766166,1.47046690225272,-0.153903532139401));
#18992=CARTESIAN_POINT('Ctrl Pts',(7.10293707314934,1.4053649764002,-0.158120627745664));
#18993=CARTESIAN_POINT('Ctrl Pts',(7.14854350112589,1.33780380077203,-0.162337723351927));
#18994=CARTESIAN_POINT('Ctrl Pts',(7.19067477458605,1.2681404938478,-0.166554818958191));
#18995=CARTESIAN_POINT('Ctrl Pts',(7.23280512349857,1.19847871564653,-0.170771822022609));
#18996=CARTESIAN_POINT('Ctrl Pts',(7.27146023002617,1.12671529608835,-0.174988825087027));
#18997=CARTESIAN_POINT('Ctrl Pts',(7.30643822496742,1.05323430682007,-0.179205828151446));
#18998=CARTESIAN_POINT('Ctrl Pts',(7.34156102952335,0.979449104752861,-0.183440289694827));
#18999=CARTESIAN_POINT('Ctrl Pts',(7.37297599659099,0.903932501600326,-0.187674751238211));
#19000=CARTESIAN_POINT('Ctrl Pts',(7.40052719086964,0.827094430285556,-0.191909212781592));
#19001=CARTESIAN_POINT('Ctrl Pts',(7.42800457278192,0.750462215741043,-0.196132329784928));
#19002=CARTESIAN_POINT('Ctrl Pts',(7.45163876205086,0.672516064084704,-0.200355446788263));
#19003=CARTESIAN_POINT('Ctrl Pts',(7.47132541865902,0.593676897354868,-0.204578563791598));
#19004=CARTESIAN_POINT('Ctrl Pts',(7.49109140153166,0.514520052681181,-0.208818697605003));
#19005=CARTESIAN_POINT('Ctrl Pts',(7.50687788911849,0.434463445243041,-0.213058831418408));
#19006=CARTESIAN_POINT('Ctrl Pts',(7.51863154107017,0.353940590342874,-0.217298965231812));
#19007=CARTESIAN_POINT('Ctrl Pts',(7.53038519302186,0.2734177354427,-0.221539099045217));
#19008=CARTESIAN_POINT('Ctrl Pts',(7.53810602691446,0.192429104206554,-0.225779232858622));
#19009=CARTESIAN_POINT('Ctrl Pts',(7.54179332448114,0.111408641021281,-0.230019366672027));
#19010=CARTESIAN_POINT('Ctrl Pts',(7.54347186327011,0.0745263477708464,
-0.231949568655315));
#19011=CARTESIAN_POINT('Ctrl Pts',(7.54431692344925,0.0376058353287048,
-0.233879770638604));
#19012=CARTESIAN_POINT('Ctrl Pts',(7.54432706310245,0.000672763404615103,
-0.235809972621892));
#19013=CARTESIAN_POINT('',(7.54432655273177,0.00171870210940699,-1.03580994220875));
#19014=CARTESIAN_POINT('Ctrl Pts',(7.54432706310264,0.000672762683487049,
-0.235809972659579));
#19015=CARTESIAN_POINT('Ctrl Pts',(7.54434913504306,-0.0797230281083711,
-0.240011630056277));
#19016=CARTESIAN_POINT('Ctrl Pts',(7.54041051570088,-0.160277450484104,
-0.244213287452976));
#19017=CARTESIAN_POINT('Ctrl Pts',(7.53249050506246,-0.2405645802526,-0.248414944849674));
#19018=CARTESIAN_POINT('Ctrl Pts',(7.52458159021619,-0.320739229199403,
-0.252610715800091));
#19019=CARTESIAN_POINT('Ctrl Pts',(7.51270240427678,-0.400646863270127,
-0.256806486750507));
#19020=CARTESIAN_POINT('Ctrl Pts',(7.496884261858,-0.479861223018667,-0.261002257700924));
#19021=CARTESIAN_POINT('Ctrl Pts',(7.48108343481782,-0.55898887052289,-0.265193435737671));
#19022=CARTESIAN_POINT('Ctrl Pts',(7.46135230928154,-0.637424290794586,
-0.269384613774418));
#19023=CARTESIAN_POINT('Ctrl Pts',(7.43777386554803,-0.714747556998403,
-0.273575791811165));
#19024=CARTESIAN_POINT('Ctrl Pts',(7.41420923082477,-0.792025537865028,
-0.277764515232116));
#19025=CARTESIAN_POINT('Ctrl Pts',(7.38680188651064,-0.868192206759783,
-0.281953238653067));
#19026=CARTESIAN_POINT('Ctrl Pts',(7.35568533976997,-0.942840285540893,
-0.286141962074018));
#19027=CARTESIAN_POINT('Ctrl Pts',(7.32457715080191,-1.01746831416433,-0.290329560421606));
#19028=CARTESIAN_POINT('Ctrl Pts',(7.2897619191426,-1.09057812712337,-0.294517158769195));
#19029=CARTESIAN_POINT('Ctrl Pts',(7.25142167462247,-1.16178145141431,-0.298704757116783));
#19030=CARTESIAN_POINT('Ctrl Pts',(7.21307957177671,-1.23298822688205,-0.302892558434421));
#19031=CARTESIAN_POINT('Ctrl Pts',(7.17121234244279,-1.30228791558973,-0.307080359752057));
#19032=CARTESIAN_POINT('Ctrl Pts',(7.12604771747784,-1.3693172887552,-0.311268161069695));
#19033=CARTESIAN_POINT('Ctrl Pts',(7.08083722339339,-1.43641473684281,-0.315460215511524));
#19034=CARTESIAN_POINT('Ctrl Pts',(7.03232291287187,-1.50123687440294,-0.319652269953352));
#19035=CARTESIAN_POINT('Ctrl Pts',(6.98077516759411,-1.56345049473181,-0.323844324395181));
#19036=CARTESIAN_POINT('Ctrl Pts',(6.92919923522328,-1.62569813441685,-0.328038671116295));
#19037=CARTESIAN_POINT('Ctrl Pts',(6.87458688596316,-1.6853340702272,-0.332233017837412));
#19038=CARTESIAN_POINT('Ctrl Pts',(6.81724628663476,-1.74206106330321,-0.336427364558526));
#19039=CARTESIAN_POINT('Ctrl Pts',(6.75980868398242,-1.79888402166297,-0.340628806872962));
#19040=CARTESIAN_POINT('Ctrl Pts',(6.69963396885148,-1.85278789833906,-0.344830249187399));
#19041=CARTESIAN_POINT('Ctrl Pts',(6.6370639836603,-1.90351525921518,-0.349031691501835));
#19042=CARTESIAN_POINT('Ctrl Pts',(6.59826927250458,-1.93496729339527,-0.351636674394639));
#19043=CARTESIAN_POINT('Ctrl Pts',(6.55855437060663,-1.96519902747761,-0.354241657287441));
#19044=CARTESIAN_POINT('Ctrl Pts',(6.51800593252828,-1.99415773220894,-0.356846640180244));
#19045=CARTESIAN_POINT('Ctrl Pts',(6.45213040376664,-2.04120442689893,-0.361078729839206));
#19046=CARTESIAN_POINT('Ctrl Pts',(6.38379825808443,-2.08507115137392,-0.365310819498166));
#19047=CARTESIAN_POINT('Ctrl Pts',(6.31334926780181,-2.12549195893388,-0.369542909157127));
#19048=CARTESIAN_POINT('Ctrl Pts',(6.24300096595243,-2.16585499550567,-0.373768950149169));
#19049=CARTESIAN_POINT('Ctrl Pts',(6.17054222811684,-2.20278166749751,-0.377994991141211));
#19050=CARTESIAN_POINT('Ctrl Pts',(6.096343142351,-2.2360482879433,-0.382221032133253));
#19051=CARTESIAN_POINT('Ctrl Pts',(6.02212364753813,-2.26932405863688,-0.386448235531387));
#19052=CARTESIAN_POINT('Ctrl Pts',(5.94616324199017,-2.29893751481338,-0.390675438929521));
#19053=CARTESIAN_POINT('Ctrl Pts',(5.86885846270999,-2.32471002982559,-0.394902642327654));
#19054=CARTESIAN_POINT('Ctrl Pts',(5.79171323148945,-2.35042935336891,-0.399121121270377));
#19055=CARTESIAN_POINT('Ctrl Pts',(5.7132296032131,-2.37232340372829,-0.4033396002131));
#19056=CARTESIAN_POINT('Ctrl Pts',(5.63382147251977,-2.3902628281291,-0.407558079155823));
#19057=CARTESIAN_POINT('Ctrl Pts',(5.5544393815825,-2.40819636977922,-0.411775174762083));
#19058=CARTESIAN_POINT('Ctrl Pts',(5.47413384320326,-2.42217775850318,-0.415992270368343));
#19059=CARTESIAN_POINT('Ctrl Pts',(5.39333155282869,-2.43212815574194,-0.420209365974603));
#19060=CARTESIAN_POINT('Ctrl Pts',(5.31253103561598,-2.4420783346247,-0.424426369039018));
#19061=CARTESIAN_POINT('Ctrl Pts',(5.23123424942722,-2.4479976422455,-0.428643372103433));
#19062=CARTESIAN_POINT('Ctrl Pts',(5.14987423853903,-2.44985897032412,-0.432860375167848));
#19063=CARTESIAN_POINT('Ctrl Pts',(5.06817739554108,-2.45172800433907,-0.437094836711232));
#19064=CARTESIAN_POINT('Ctrl Pts',(4.98641727461081,-2.44950536333501,-0.441329298254615));
#19065=CARTESIAN_POINT('Ctrl Pts',(4.90503173005962,-2.44321643276859,-0.445563759798));
#19066=CARTESIAN_POINT('Ctrl Pts',(4.823864225408,-2.43694435086733,-0.449786876801334));
#19067=CARTESIAN_POINT('Ctrl Pts',(4.74306975123904,-2.42662783962602,-0.45400999380467));
#19068=CARTESIAN_POINT('Ctrl Pts',(4.66307508507545,-2.41234386103336,-0.458233110808004));
#19069=CARTESIAN_POINT('Ctrl Pts',(4.58275808494858,-2.39800232596035,-0.462473244621414));
#19070=CARTESIAN_POINT('Ctrl Pts',(4.50324780944176,-2.37966139703956,-0.466713378434822));
#19071=CARTESIAN_POINT('Ctrl Pts',(4.42496166673162,-2.35744972544429,-0.470953512248231));
#19072=CARTESIAN_POINT('Ctrl Pts',(4.34667552402147,-2.33523805384901,-0.47519364606164));
#19073=CARTESIAN_POINT('Ctrl Pts',(4.26961393682897,-2.30915584832712,-0.47943377987505));
#19074=CARTESIAN_POINT('Ctrl Pts',(4.19417318033833,-2.27937995407966,-0.48367391368846));
#19075=CARTESIAN_POINT('Ctrl Pts',(4.11887554600458,-2.2496605490617,-0.487906003347422));
#19076=CARTESIAN_POINT('Ctrl Pts',(4.04491167209826,-2.21615059522003,-0.492138093006385));
#19077=CARTESIAN_POINT('Ctrl Pts',(3.97268947649545,-2.17899071930594,-0.496370182665347));
#19078=CARTESIAN_POINT('Ctrl Pts',(3.90057050365971,-2.1418839537298,-0.500596223657394));
#19079=CARTESIAN_POINT('Ctrl Pts',(3.83018867490804,-2.10113783766085,-0.50482226464944));
#19080=CARTESIAN_POINT('Ctrl Pts',(3.76193291616568,-2.05694141514846,-0.509048305641486));
#19081=CARTESIAN_POINT('Ctrl Pts',(3.69365838313564,-2.0127328360596,-0.513275509039619));
#19082=CARTESIAN_POINT('Ctrl Pts',(3.62751151362544,-1.96507224802579,-0.517502712437752));
#19083=CARTESIAN_POINT('Ctrl Pts',(3.56385778900744,-1.9141953891225,-0.521729915835885));
#19084=CARTESIAN_POINT('Ctrl Pts',(3.50033543826238,-1.86342353412962,-0.525948394778608));
#19085=CARTESIAN_POINT('Ctrl Pts',(3.4392963301879,-1.80944894164363,-0.530166873721331));
#19086=CARTESIAN_POINT('Ctrl Pts',(3.3810740230668,-1.75254870331779,-0.534385352664054));
#19087=CARTESIAN_POINT('Ctrl Pts',(3.32287080838197,-1.6956671238914,-0.538602448270314));
#19088=CARTESIAN_POINT('Ctrl Pts',(3.26748289235775,-1.63586212841842,-0.542819543876574));
#19089=CARTESIAN_POINT('Ctrl Pts',(3.21520839209312,-1.5734490115513,-0.547036639482834));
#19090=CARTESIAN_POINT('Ctrl Pts',(3.16293503896367,-1.51103726430574,-0.551253642547249));
#19091=CARTESIAN_POINT('Ctrl Pts',(3.11377526324356,-1.44601786644264,-0.555470645611663));
#19092=CARTESIAN_POINT('Ctrl Pts',(3.06798721296626,-1.37873956112997,-0.559687648676078));
#19093=CARTESIAN_POINT('Ctrl Pts',(3.02200959922396,-1.31118272225676,-0.563922110219461));
#19094=CARTESIAN_POINT('Ctrl Pts',(2.97943196451938,-1.24134861504167,-0.568156571762844));
#19095=CARTESIAN_POINT('Ctrl Pts',(2.94047101054731,-1.16961855457087,-0.572391033306228));
#19096=CARTESIAN_POINT('Ctrl Pts',(2.90161443681301,-1.09808066600562,-0.576614150309561));
#19097=CARTESIAN_POINT('Ctrl Pts',(2.8663553549631,-1.02465740942075,-0.580837267312894));
#19098=CARTESIAN_POINT('Ctrl Pts',(2.83486115444521,-0.949748838530668,
-0.585060384316227));
#19099=CARTESIAN_POINT('Ctrl Pts',(2.80324004983532,-0.874538427809293,
-0.589300518129635));
#19100=CARTESIAN_POINT('Ctrl Pts',(2.7754143840211,-0.797831153663746,-0.593540651943045));
#19101=CARTESIAN_POINT('Ctrl Pts',(2.75150306778021,-0.720047302826222,
-0.597780785756453));
#19102=CARTESIAN_POINT('Ctrl Pts',(2.72759175153932,-0.642263451988699,
-0.602020919569861));
#19103=CARTESIAN_POINT('Ctrl Pts',(2.70759483944076,-0.563403492744268,
-0.606261053383269));
#19104=CARTESIAN_POINT('Ctrl Pts',(2.69157930278517,-0.48389617104529,-0.610501187196677));
#19105=CARTESIAN_POINT('Ctrl Pts',(2.67559414994672,-0.404539686372571,
-0.614733276855639));
#19106=CARTESIAN_POINT('Ctrl Pts',(2.66351562688312,-0.324242233546837,
-0.618965366514602));
#19107=CARTESIAN_POINT('Ctrl Pts',(2.65544743384368,-0.243422643243998,
-0.623197456173564));
#19108=CARTESIAN_POINT('Ctrl Pts',(2.64739077217912,-0.162718563438931,
-0.627423497165596));
#19109=CARTESIAN_POINT('Ctrl Pts',(2.64333310249612,-0.0814942868349896,
-0.631649538157628));
#19110=CARTESIAN_POINT('Ctrl Pts',(2.64332716199235,-0.00017902179174532,
-0.63587557914966));
#19111=CARTESIAN_POINT('Ctrl Pts',(2.6433212198546,0.0811586096602686,-0.640102782547795));
#19112=CARTESIAN_POINT('Ctrl Pts',(2.64736930210408,0.162586817474471,-0.644329985945929));
#19113=CARTESIAN_POINT('Ctrl Pts',(2.65547220897854,0.243670689667399,-0.648557189344064));
#19114=CARTESIAN_POINT('Ctrl Pts',(2.66355839239706,0.324587214193079,-0.652775668286786));
#19115=CARTESIAN_POINT('Ctrl Pts',(2.67568265845103,0.405160358113423,-0.656994147229508));
#19116=CARTESIAN_POINT('Ctrl Pts',(2.69179374419152,0.48495952530394,-0.66121262617223));
#19117=CARTESIAN_POINT('Ctrl Pts',(2.70789954673575,0.564732524508723,-0.6654297217785));
#19118=CARTESIAN_POINT('Ctrl Pts',(2.72798948075679,0.643731595870925,-0.66964681738477));
#19119=CARTESIAN_POINT('Ctrl Pts',(2.75196095221086,0.721535124655565,-0.67386391299104));
#19120=CARTESIAN_POINT('Ctrl Pts',(2.77593189762414,0.799336946084448,-0.678080916055461));
#19121=CARTESIAN_POINT('Ctrl Pts',(2.80378407319052,0.875942833348865,-0.682297919119882));
#19122=CARTESIAN_POINT('Ctrl Pts',(2.835365083211,0.950946538057679,-0.686514922184302));
#19123=CARTESIAN_POINT('Ctrl Pts',(2.86707683925908,1.02626075963848,-0.690749383727684));
#19124=CARTESIAN_POINT('Ctrl Pts',(2.90254819921196,1.09995906444025,-0.694983845271068));
#19125=CARTESIAN_POINT('Ctrl Pts',(2.94157689847623,1.17165228687651,-0.69921830681445));
#19126=CARTESIAN_POINT('Ctrl Pts',(2.98050103600642,1.24315343609995,-0.703441423817783));
#19127=CARTESIAN_POINT('Ctrl Pts',(3.02296319736942,1.31265985532011,-0.707664540821115));
#19128=CARTESIAN_POINT('Ctrl Pts',(3.06871858438887,1.37981358356922,-0.711887657824448));
#19129=CARTESIAN_POINT('Ctrl Pts',(3.11465834014121,1.44723790395171,-0.716127791637856));
#19130=CARTESIAN_POINT('Ctrl Pts',(3.16391762583028,1.51229016262306,-0.720367925451264));
#19131=CARTESIAN_POINT('Ctrl Pts',(3.21620830848705,1.57464209124418,-0.724608059264671));
#19132=CARTESIAN_POINT('Ctrl Pts',(3.26849899114382,1.6369940198653,-0.728848193078079));
#19133=CARTESIAN_POINT('Ctrl Pts',(3.32382070737263,1.69664531808261,-0.733088326891487));
#19134=CARTESIAN_POINT('Ctrl Pts',(3.38184999060225,1.75330671504709,-0.737328460704894));
#19135=CARTESIAN_POINT('Ctrl Pts',(3.43976918378819,1.80986061704834,-0.741560550363855));
#19136=CARTESIAN_POINT('Ctrl Pts',(3.50060175364413,1.86364695448099,-0.745792640022815));
#19137=CARTESIAN_POINT('Ctrl Pts',(3.56405252120228,1.91435101755209,-0.750024729681776));
#19138=CARTESIAN_POINT('Ctrl Pts',(3.62741260245896,1.96498261240688,-0.754250770673819));
#19139=CARTESIAN_POINT('Ctrl Pts',(3.69338308935504,2.01254039464928,-0.758476811665862));
#19140=CARTESIAN_POINT('Ctrl Pts',(3.76163238981095,2.05674678956736,-0.762702852657904));
#19141=CARTESIAN_POINT('Ctrl Pts',(3.82990046277823,2.10096534380495,-0.766930056056037));
#19142=CARTESIAN_POINT('Ctrl Pts',(3.90044825105633,2.14183036022238,-0.771157259454171));
#19143=CARTESIAN_POINT('Ctrl Pts',(3.97291114326049,2.17910475737404,-0.775384462852305));
#19144=CARTESIAN_POINT('Ctrl Pts',(4.04522448049597,2.21630222451189,-0.77960294179503));
#19145=CARTESIAN_POINT('Ctrl Pts',(4.11944462263436,2.24992364401679,-0.783821420737755));
#19146=CARTESIAN_POINT('Ctrl Pts',(4.19518228029349,2.27977798005625,-0.78803989968048));
#19147=CARTESIAN_POINT('Ctrl Pts',(4.2708951018292,2.30962252617089,-0.792256995286739));
#19148=CARTESIAN_POINT('Ctrl Pts',(4.34812401866058,2.3357022717617,-0.796474090892998));
#19149=CARTESIAN_POINT('Ctrl Pts',(4.4264593774043,2.35787414821533,-0.800691186499257));
#19150=CARTESIAN_POINT('Ctrl Pts',(4.50479301712181,2.38004553811938,-0.804908189563682));
#19151=CARTESIAN_POINT('Ctrl Pts',(4.58423260303908,2.39830910394468,-0.809125192628107));
#19152=CARTESIAN_POINT('Ctrl Pts',(4.66435430840104,2.4125719312893,-0.813342195692531));
#19153=CARTESIAN_POINT('Ctrl Pts',(4.74480771926232,2.42689380703092,-0.817576657235913));
#19154=CARTESIAN_POINT('Ctrl Pts',(4.82594844733252,2.43718165208201,-0.821811118779293));
#19155=CARTESIAN_POINT('Ctrl Pts',(4.9073398966582,2.44339369572469,-0.826045580322675));
#19156=CARTESIAN_POINT('Ctrl Pts',(4.98851329026488,2.44958909668986,-0.830268697326008));
#19157=CARTESIAN_POINT('Ctrl Pts',(5.06993559493242,2.45173053617133,-0.834491814329344));
#19158=CARTESIAN_POINT('Ctrl Pts',(5.15117328608491,2.44982890653645,-0.838714931332677));
#19159=CARTESIAN_POINT('Ctrl Pts',(5.23273831989921,2.44791961439297,-0.842955065146082));
#19160=CARTESIAN_POINT('Ctrl Pts',(5.31411677973302,2.44193464489328,-0.847195198959485));
#19161=CARTESIAN_POINT('Ctrl Pts',(5.39487650776651,2.43193740410227,-0.851435332772891));
#19162=CARTESIAN_POINT('Ctrl Pts',(5.47563623579999,2.42194016331125,-0.855675466586296));
#19163=CARTESIAN_POINT('Ctrl Pts',(5.55577678239443,2.40793079298116,-0.859915600399702));
#19164=CARTESIAN_POINT('Ctrl Pts',(5.63487951587856,2.39002355496301,-0.864155734213107));
#19165=CARTESIAN_POINT('Ctrl Pts',(5.71383217989943,2.37215028959638,-0.868387823872063));
#19166=CARTESIAN_POINT('Ctrl Pts',(5.79204552480634,2.35032726670422,-0.872619913531017));
#19167=CARTESIAN_POINT('Ctrl Pts',(5.86909494316994,2.32463117662322,-0.876852003189972));
#19168=CARTESIAN_POINT('Ctrl Pts',(5.94603423951238,2.29897181239214,-0.881078044182022));
#19169=CARTESIAN_POINT('Ctrl Pts',(6.02181247612417,2.26945052093748,-0.885304085174071));
#19170=CARTESIAN_POINT('Ctrl Pts',(6.096016421698,2.23619474210623,-0.88953012616612));
#19171=CARTESIAN_POINT('Ctrl Pts',(6.17024077765544,2.20292981600931,-0.893757329564254));
#19172=CARTESIAN_POINT('Ctrl Pts',(6.2428895277158,2.16592847667684,-0.897984532962389));
#19173=CARTESIAN_POINT('Ctrl Pts',(6.31356548021765,2.12536789029584,-0.902211736360522));
#19174=CARTESIAN_POINT('Ctrl Pts',(6.38409556578601,2.08489101624055,-0.906430215303235));
#19175=CARTESIAN_POINT('Ctrl Pts',(6.45266057340775,2.04086978183757,-0.910648694245948));
#19176=CARTESIAN_POINT('Ctrl Pts',(6.51888854564184,1.99352709642818,-0.914867173188661));
#19177=CARTESIAN_POINT('Ctrl Pts',(6.58509480019769,1.94619993577629,-0.919084268794919));
#19178=CARTESIAN_POINT('Ctrl Pts',(6.64896516356175,1.8955537571567,-0.923301364401177));
#19179=CARTESIAN_POINT('Ctrl Pts',(6.71015687043186,1.84185463663035,-0.927518460007435));
#19180=CARTESIAN_POINT('Ctrl Pts',(6.77134723448354,1.78815669450173,-0.931735463071845));
#19181=CARTESIAN_POINT('Ctrl Pts',(6.82985871040158,1.73140625103906,-0.935952466136255));
#19182=CARTESIAN_POINT('Ctrl Pts',(6.88538292579639,1.67190854168214,-0.940169469200665));
#19183=CARTESIAN_POINT('Ctrl Pts',(6.94113701257911,1.612164510591,-0.944403930744053));
#19184=CARTESIAN_POINT('Ctrl Pts',(6.9938787201965,1.54965075382351,-0.948638392287441));
#19185=CARTESIAN_POINT('Ctrl Pts',(7.04333566297374,1.48471102545401,-0.952872853830829));
#19186=CARTESIAN_POINT('Ctrl Pts',(7.09266010572405,1.41994527702087,-0.957095970834159));
#19187=CARTESIAN_POINT('Ctrl Pts',(7.13871713113911,1.35276694814664,-0.961319087837489));
#19188=CARTESIAN_POINT('Ctrl Pts',(7.18128022621014,1.28354584156043,-0.965542204840819));
#19189=CARTESIAN_POINT('Ctrl Pts',(7.22401482685513,1.21404581245705,-0.969782338654237));
#19190=CARTESIAN_POINT('Ctrl Pts',(7.26322706153343,1.14248692596204,-0.974022472467655));
#19191=CARTESIAN_POINT('Ctrl Pts',(7.29873523791343,1.0692663830408,-0.978262606281072));
#19192=CARTESIAN_POINT('Ctrl Pts',(7.33424341429343,0.996045840119555,-0.98250274009449));
#19193=CARTESIAN_POINT('Ctrl Pts',(7.36604740694091,0.921164095233241,-0.986742873907906));
#19194=CARTESIAN_POINT('Ctrl Pts',(7.39401556223305,0.845034640304858,-0.990983007721324));
#19195=CARTESIAN_POINT('Ctrl Pts',(7.42616850853459,0.757514163866223,-0.995857580012206));
#19196=CARTESIAN_POINT('Ctrl Pts',(7.45335219664486,0.668075732514126,-1.00073215230309));
#19197=CARTESIAN_POINT('Ctrl Pts',(7.47536636025791,0.577253207853991,-1.00560672459397));
#19198=CARTESIAN_POINT('Ctrl Pts',(7.49809992997903,0.483462672228753,-1.01064059419644));
#19199=CARTESIAN_POINT('Ctrl Pts',(7.51532012506383,0.388196137853416,-1.0156744637989));
#19200=CARTESIAN_POINT('Ctrl Pts',(7.52685978595101,0.292065864031482,-1.02070833340136));
#19201=CARTESIAN_POINT('Ctrl Pts',(7.53839944683819,0.195935590209548,-1.02574220300383));
#19202=CARTESIAN_POINT('Ctrl Pts',(7.54425836357575,0.098941766422127,-1.03077607260629));
#19203=CARTESIAN_POINT('Ctrl Pts',(7.54432655273177,0.00171870210940699,
-1.03580994220875));
#19204=CARTESIAN_POINT('',(7.54195689531145,-0.00183542994100908,-1.83580997262189));
#19205=CARTESIAN_POINT('Ctrl Pts',(7.54168867809974,0.00171626522762203,
-1.03580997262189));
#19206=CARTESIAN_POINT('Ctrl Pts',(7.53826864661413,-0.525630169298386,
-1.06314340882444));
#19207=CARTESIAN_POINT('Ctrl Pts',(7.11247511815589,-1.87364194780338,-1.13275260286306));
#19208=CARTESIAN_POINT('Ctrl Pts',(4.8932778873185,-2.88797071625038,-1.24463755473777));
#19209=CARTESIAN_POINT('Ctrl Pts',(2.56077426740912,-1.4015127303073,-1.37146482824597));
#19210=CARTESIAN_POINT('Ctrl Pts',(2.54053909816163,1.36430017347163,-1.4982921017542));
#19211=CARTESIAN_POINT('Ctrl Pts',(4.85104382313895,2.88472721769187,-1.62511937526241));
#19212=CARTESIAN_POINT('Ctrl Pts',(7.09724317847486,1.89752826528236,-1.7376253322183));
#19213=CARTESIAN_POINT('Ctrl Pts',(7.53818940518866,0.537343417442344,-1.80785553133814));
#19214=CARTESIAN_POINT('Ctrl Pts',(7.54195689531145,-0.00183542994100908,
-1.83580997262189));
#19215=CARTESIAN_POINT('',(7.54821176704488,-0.000461678752230058,-2.63580997262189));
#19216=CARTESIAN_POINT('Ctrl Pts',(7.54195689531145,-0.00183542994100908,
-1.83580997262189));
#19217=CARTESIAN_POINT('Ctrl Pts',(7.5438870150412,-0.278061696576387,-1.85013128917421));
#19218=CARTESIAN_POINT('Ctrl Pts',(7.37337369192932,-1.3673806984397,-1.90672836356257));
#19219=CARTESIAN_POINT('Ctrl Pts',(5.77424896835661,-2.81382675798286,-2.00560119578708));
#19220=CARTESIAN_POINT('Ctrl Pts',(3.10188638839217,-2.10065866965814,-2.13242846929526));
#19221=CARTESIAN_POINT('Ctrl Pts',(2.24784422830493,0.530071735913177,-2.2592557428035));
#19222=CARTESIAN_POINT('Ctrl Pts',(3.99172513773674,2.67693220178668,-2.38608301631169));
#19223=CARTESIAN_POINT('Ctrl Pts',(6.71326075235729,2.38324884212861,-2.51160109291785));
#19224=CARTESIAN_POINT('Ctrl Pts',(7.54617393712679,0.784506871056184,-2.5948434116879));
#19225=CARTESIAN_POINT('Ctrl Pts',(7.54821176704488,-0.000461678752230058,
-2.63580997262189));
#19226=CARTESIAN_POINT('',(7.54432619404611,0.00217068071508165,-3.43580997262189));
#19227=CARTESIAN_POINT('Ctrl Pts',(7.54821176704488,-0.000461678752230058,
-2.63580997262189));
#19228=CARTESIAN_POINT('Ctrl Pts',(7.54827689139399,-0.0255474650670082,
-2.63711916952397));
#19229=CARTESIAN_POINT('Ctrl Pts',(7.53657731044435,-0.86062535690245,-2.68070412426241));
#19230=CARTESIAN_POINT('Ctrl Pts',(6.59176122330639,-2.4772542092338,-2.7665648368361));
#19231=CARTESIAN_POINT('Ctrl Pts',(3.82877477306649,-2.60388887691698,-2.8933921103447));
#19232=CARTESIAN_POINT('Ctrl Pts',(2.22057696198272,-0.353593302260975,
-3.02021938385273));
#19233=CARTESIAN_POINT('Ctrl Pts',(3.23519284446952,2.21947595045414,-3.14704665736103));
#19234=CARTESIAN_POINT('Ctrl Pts',(5.94644184717804,2.76652176454744,-3.27387393086921));
#19235=CARTESIAN_POINT('Ctrl Pts',(7.41343420069762,1.26507933464666,-3.37012820241141));
#19236=CARTESIAN_POINT('Ctrl Pts',(7.54521044087543,0.227592873628459,-3.42410671611751));
#19237=CARTESIAN_POINT('Ctrl Pts',(7.54327308142312,0.00217939078736114,
-3.43580947198754));
#19238=CARTESIAN_POINT('',(7.54432691509248,-0.00108536048784296,-4.23580997266998));
#19239=CARTESIAN_POINT('Ctrl Pts',(7.54432619404611,0.00217068071508165,
-3.43580997262189));
#19240=CARTESIAN_POINT('Ctrl Pts',(7.54439758870441,-0.078427327229146,
-3.43999260303891));
#19241=CARTESIAN_POINT('Ctrl Pts',(7.54048835863658,-0.159110489756147,
-3.44417523345593));
#19242=CARTESIAN_POINT('Ctrl Pts',(7.53260002672682,-0.239451732796754,
-3.44835786387295));
#19243=CARTESIAN_POINT('Ctrl Pts',(7.52471552022917,-0.319754014702473,
-3.45253846594161));
#19244=CARTESIAN_POINT('Ctrl Pts',(7.51285578731776,-0.399714235521038,
-3.45671906801028));
#19245=CARTESIAN_POINT('Ctrl Pts',(7.49707436664272,-0.478908229110086,
-3.46089967007895));
#19246=CARTESIAN_POINT('Ctrl Pts',(7.48129555875154,-0.558089111282113,
-3.465079580004));
#19247=CARTESIAN_POINT('Ctrl Pts',(7.46159644547567,-0.636503553768053,
-3.46925948992905));
#19248=CARTESIAN_POINT('Ctrl Pts',(7.43808179801882,-0.713736940902685,
-3.4734393998541));
#19249=CARTESIAN_POINT('Ctrl Pts',(7.41456353334558,-0.79098220871184,-3.47761995276726));
#19250=CARTESIAN_POINT('Ctrl Pts',(7.38722870964907,-0.867045608132491,
-3.48180050568042));
#19251=CARTESIAN_POINT('Ctrl Pts',(7.35623167916053,-0.941528555652031,
-3.48598105859357));
#19252=CARTESIAN_POINT('Ctrl Pts',(7.32520084589774,-1.01609272805733,-3.4901661704688));
#19253=CARTESIAN_POINT('Ctrl Pts',(7.29050002102054,-1.08907257242188,-3.49435128234403));
#19254=CARTESIAN_POINT('Ctrl Pts',(7.25233103441385,-1.1600910544054,-3.49853639421926));
#19255=CARTESIAN_POINT('Ctrl Pts',(7.21413743471517,-1.23115533232395,-3.50272420484426));
#19256=CARTESIAN_POINT('Ctrl Pts',(7.17247146990418,-1.30025532754648,-3.50691201546925));
#19257=CARTESIAN_POINT('Ctrl Pts',(7.12757876976536,-1.36704228950033,-3.51109982609424));
#19258=CARTESIAN_POINT('Ctrl Pts',(7.08261342757628,-1.43393732118115,-3.51529441312496));
#19259=CARTESIAN_POINT('Ctrl Pts',(7.034411218612,-1.49851147622434,-3.51948900015567));
#19260=CARTESIAN_POINT('Ctrl Pts',(6.98325807161719,-1.56044899405375,-3.52368358718638));
#19261=CARTESIAN_POINT('Ctrl Pts',(6.96762854260127,-1.57937362115806,-3.52496521741947));
#19262=CARTESIAN_POINT('Ctrl Pts',(6.95172377923429,-1.59805236380879,-3.52624684765256));
#19263=CARTESIAN_POINT('Ctrl Pts',(6.93555258953373,-1.61647693316687,-3.52752847788565));
#19264=CARTESIAN_POINT('Ctrl Pts',(6.88215346160043,-1.67731697984777,-3.53176056829132));
#19265=CARTESIAN_POINT('Ctrl Pts',(6.82563677564708,-1.73562167328497,-3.53599265869699));
#19266=CARTESIAN_POINT('Ctrl Pts',(6.7662726377776,-1.7910545381569,-3.54022474910266));
#19267=CARTESIAN_POINT('Ctrl Pts',(6.70699334571578,-1.8464081759675,-3.54445079082066));
#19268=CARTESIAN_POINT('Ctrl Pts',(6.64487502140792,-1.89889782278366,-3.54867683253866));
#19269=CARTESIAN_POINT('Ctrl Pts',(6.58022693169389,-1.94822122850342,-3.55290287425666));
#19270=CARTESIAN_POINT('Ctrl Pts',(6.51556107393455,-1.99755819039339,-3.55713007747071));
#19271=CARTESIAN_POINT('Ctrl Pts',(6.4483643874204,-2.04372683776174,-3.56135728068476));
#19272=CARTESIAN_POINT('Ctrl Pts',(6.37898217397017,-2.08646275509064,-3.56558448389881));
#19273=CARTESIAN_POINT('Ctrl Pts',(6.3097431432978,-2.12911047910524,-3.56980296351255));
#19274=CARTESIAN_POINT('Ctrl Pts',(6.23832797971304,-2.16833936204582,-3.5740214431263));
#19275=CARTESIAN_POINT('Ctrl Pts',(6.16511013077376,-2.20392899994263,-3.57823992274004));
#19276=CARTESIAN_POINT('Ctrl Pts',(6.0919162920328,-2.23950696699311,-3.5824570189953));
#19277=CARTESIAN_POINT('Ctrl Pts',(6.01692135951845,-2.27144785601514,-3.58667411525056));
#19278=CARTESIAN_POINT('Ctrl Pts',(5.94052277285294,-2.29957752238882,-3.59089121150582));
#19279=CARTESIAN_POINT('Ctrl Pts',(5.8641258631243,-2.32770657132079,-3.59510821519649));
#19280=CARTESIAN_POINT('Ctrl Pts',(5.78632579696908,-2.3520244044536,-3.59932521888716));
#19281=CARTESIAN_POINT('Ctrl Pts',(5.70753800193967,-2.37240579305159,-3.60354222257783));
#19282=CARTESIAN_POINT('Ctrl Pts',(5.62842405068523,-2.39287155406746,-3.6077766833125));
#19283=CARTESIAN_POINT('Ctrl Pts',(5.548314628918,-2.40936807926592,-3.61201114404717));
#19284=CARTESIAN_POINT('Ctrl Pts',(5.46764182775742,-2.42182015037658,-3.61624560478184));
#19285=CARTESIAN_POINT('Ctrl Pts',(5.38718513085923,-2.43423886519361,-3.62046872235003));
#19286=CARTESIAN_POINT('Ctrl Pts',(5.30616853837484,-2.44263475937152,-3.62469183991823));
#19287=CARTESIAN_POINT('Ctrl Pts',(5.22502512900846,-2.44698535789141,-3.62891495748642));
#19288=CARTESIAN_POINT('Ctrl Pts',(5.14355479651501,-2.45135348477601,-3.63315508980433));
#19289=CARTESIAN_POINT('Ctrl Pts',(5.06195709457774,-2.45164365752016,-3.63739522212224));
#19290=CARTESIAN_POINT('Ctrl Pts',(4.98066777652398,-2.44788586436549,-3.64163535444015));
#19291=CARTESIAN_POINT('Ctrl Pts',(4.89937845847021,-2.44412807121081,-3.64587548675806));
#19292=CARTESIAN_POINT('Ctrl Pts',(4.81839798350605,-2.43632241891511,-3.65011561907597));
#19293=CARTESIAN_POINT('Ctrl Pts',(4.73815252936359,-2.42455064091392,-3.65435575139387));
#19294=CARTESIAN_POINT('Ctrl Pts',(4.65805914462597,-2.41280117105832,-3.65858784843546));
#19295=CARTESIAN_POINT('Ctrl Pts',(4.5783991872543,-2.39705677532944,-3.66281994547704));
#19296=CARTESIAN_POINT('Ctrl Pts',(4.49960190571245,-2.37736126883792,-3.66705204251862));
#19297=CARTESIAN_POINT('Ctrl Pts',(4.42091724336842,-2.35769391169493,-3.67127809093308));
#19298=CARTESIAN_POINT('Ctrl Pts',(4.34309325511306,-2.3340867711541,-3.67550413934755));
#19299=CARTESIAN_POINT('Ctrl Pts',(4.26655174911285,-2.30663513631102,-3.67973018776201));
#19300=CARTESIAN_POINT('Ctrl Pts',(4.18998935775338,-2.27917601092737,-3.68395738930952));
#19301=CARTESIAN_POINT('Ctrl Pts',(4.11471060589362,-2.24787038687307,-3.68818459085702));
#19302=CARTESIAN_POINT('Ctrl Pts',(4.04112513035319,-2.21286436465287,-3.69241179240452));
#19303=CARTESIAN_POINT('Ctrl Pts',(3.96769136457852,-2.1779305136783,-3.69663027881155));
#19304=CARTESIAN_POINT('Ctrl Pts',(3.89594433049418,-2.13931168443951,-3.70084876521857));
#19305=CARTESIAN_POINT('Ctrl Pts',(3.82627202538661,-2.09720152637797,-3.7050672516256));
#19306=CARTESIAN_POINT('Ctrl Pts',(3.75662256740782,-2.05510517719219,-3.70928435469527));
#19307=CARTESIAN_POINT('Ctrl Pts',(3.68904688467489,-2.00952001300304,-3.71350145776494));
#19308=CARTESIAN_POINT('Ctrl Pts',(3.62390718793589,-1.96068496681496,-3.71771856083461));
#19309=CARTESIAN_POINT('Ctrl Pts',(3.55876892081949,-1.9118509924109,-3.72193557135141));
#19310=CARTESIAN_POINT('Ctrl Pts',(3.49606690451329,-1.85976755748095,-3.72615258186821));
#19311=CARTESIAN_POINT('Ctrl Pts',(3.4361320697381,-1.8047152830284,-3.73036959238501));
#19312=CARTESIAN_POINT('Ctrl Pts',(3.37594933542629,-1.74943530404681,-3.73460404509476));
#19313=CARTESIAN_POINT('Ctrl Pts',(3.3185570784769,-1.69116218383102,-3.73883849780452));
#19314=CARTESIAN_POINT('Ctrl Pts',(3.26425330789796,-1.63021771133253,-3.74307295051428));
#19315=CARTESIAN_POINT('Ctrl Pts',(3.21009481524181,-1.56943628250992,-3.74729607486714));
#19316=CARTESIAN_POINT('Ctrl Pts',(3.1590085661019,-1.50599816639619,-3.75151919922));
#19317=CARTESIAN_POINT('Ctrl Pts',(3.11124883911793,-1.44025465442662,-3.75574232357287));
#19318=CARTESIAN_POINT('Ctrl Pts',(3.06329694188728,-1.37424661106816,-3.75998244046107));
#19319=CARTESIAN_POINT('Ctrl Pts',(3.01869864343333,-1.30591497987846,-3.76422255734928));
#19320=CARTESIAN_POINT('Ctrl Pts',(2.97766563770153,-1.23564180925838,-3.76846267423748));
#19321=CARTESIAN_POINT('Ctrl Pts',(2.93663263196972,-1.16536863863829,-3.77270279112568));
#19322=CARTESIAN_POINT('Ctrl Pts',(2.89916507896408,-1.09315437204353,-3.77694290801389));
#19323=CARTESIAN_POINT('Ctrl Pts',(2.86542603589723,-1.01940114791091,-3.78118302490209));
#19324=CARTESIAN_POINT('Ctrl Pts',(2.83175100953722,-0.945787863684691,
-3.78541509656153));
#19325=CARTESIAN_POINT('Ctrl Pts',(2.80166470736299,-0.870366825716182,
-3.78964716822096));
#19326=CARTESIAN_POINT('Ctrl Pts',(2.7753636846141,-0.793522138560183,-3.7938792398804));
#19327=CARTESIAN_POINT('Ctrl Pts',(2.74910025251282,-0.716787281412822,
-3.79810526286576));
#19328=CARTESIAN_POINT('Ctrl Pts',(2.72661150401748,-0.638633252283635,
-3.80233128585113));
#19329=CARTESIAN_POINT('Ctrl Pts',(2.708046745083,-0.559465891269729,-3.80655730883649));
#19330=CARTESIAN_POINT('Ctrl Pts',(2.68947678086819,-0.480276332913594,
-3.8107845167354));
#19331=CARTESIAN_POINT('Ctrl Pts',(2.67483317674379,-0.400073309224773,
-3.81501172463431));
#19332=CARTESIAN_POINT('Ctrl Pts',(2.664215975812,-0.31928007417146,-3.81923893253322));
#19333=CARTESIAN_POINT('Ctrl Pts',(2.65362074377035,-0.23865401479058,-3.82345739358194));
#19334=CARTESIAN_POINT('Ctrl Pts',(2.64703535420249,-0.157440641622429,
-3.82767585463066));
#19335=CARTESIAN_POINT('Ctrl Pts',(2.64450817442951,-0.0760708827182392,
-3.83189431567939));
#19336=CARTESIAN_POINT('Ctrl Pts',(2.64198182333156,0.00527219463054879,
-3.8361113934734));
#19337=CARTESIAN_POINT('Ctrl Pts',(2.64351105377966,0.086771091768486,-3.84032847126741));
#19338=CARTESIAN_POINT('Ctrl Pts',(2.64909220696122,0.167991909395576,-3.84454554906143));
#19339=CARTESIAN_POINT('Ctrl Pts',(2.6546732378064,0.249210946698602,-3.84876253441898));
#19340=CARTESIAN_POINT('Ctrl Pts',(2.66430598179138,0.330151453089001,-3.85297951977653));
#19341=CARTESIAN_POINT('Ctrl Pts',(2.67793478577229,0.410383123578419,-3.85719650513408));
#19342=CARTESIAN_POINT('Ctrl Pts',(2.69162013935566,0.490947697019378,-3.8614309879071));
#19343=CARTESIAN_POINT('Ctrl Pts',(2.70933471895357,0.5707970723659,-3.86566547068012));
#19344=CARTESIAN_POINT('Ctrl Pts',(2.73097041667715,0.649506183204621,-3.86989995345314));
#19345=CARTESIAN_POINT('Ctrl Pts',(2.75254795380765,0.728003709992476,-3.87412305318538));
#19346=CARTESIAN_POINT('Ctrl Pts',(2.7780253693176,0.80536666366508,-3.87834615291761));
#19347=CARTESIAN_POINT('Ctrl Pts',(2.80724602517311,0.881190663050533,-3.88256925264985));
#19348=CARTESIAN_POINT('Ctrl Pts',(2.83658482407696,0.957321229080808,-3.88680942694326));
#19349=CARTESIAN_POINT('Ctrl Pts',(2.86969699717403,1.03189994260836,-3.89104960123667));
#19350=CARTESIAN_POINT('Ctrl Pts',(2.906376929941,1.10454142561836,-3.89528977553008));
#19351=CARTESIAN_POINT('Ctrl Pts',(2.94305686270798,1.17718290862836,-3.89952994982349));
#19352=CARTESIAN_POINT('Ctrl Pts',(2.98330426986581,1.24788678572931,-3.90377012411689));
#19353=CARTESIAN_POINT('Ctrl Pts',(3.02687023321737,1.31629758475116,-3.9080102984103));
#19354=CARTESIAN_POINT('Ctrl Pts',(3.07035323817815,1.38457811579862,-3.91224239855571));
#19355=CARTESIAN_POINT('Ctrl Pts',(3.11730439187291,1.45082905363251,-3.91647449870111));
#19356=CARTESIAN_POINT('Ctrl Pts',(3.16750813305921,1.51467662356142,-3.92070659884652));
#19357=CARTESIAN_POINT('Ctrl Pts',(3.21764011974826,1.57843293833338,-3.92493265019534));
#19358=CARTESIAN_POINT('Ctrl Pts',(3.27101517605462,1.63979234535314,-3.92915870154416));
#19359=CARTESIAN_POINT('Ctrl Pts',(3.32737381319896,1.69840891414263,-3.93338475289298));
#19360=CARTESIAN_POINT('Ctrl Pts',(3.38374777933176,1.7570414260555,-3.93761195368571));
#19361=CARTESIAN_POINT('Ctrl Pts',(3.44310667674929,1.81292922866238,-3.94183915447844));
#19362=CARTESIAN_POINT('Ctrl Pts',(3.50514962968871,1.86575828261088,-3.94606635527117));
#19363=CARTESIAN_POINT('Ctrl Pts',(3.56706471771255,1.91847846065643,-3.95028484418533));
#19364=CARTESIAN_POINT('Ctrl Pts',(3.63165247150197,1.96815216474818,-3.95450333309948));
#19365=CARTESIAN_POINT('Ctrl Pts',(3.69857747673012,2.01450455050948,-3.95872182201364));
#19366=CARTESIAN_POINT('Ctrl Pts',(3.76548053312411,2.06084173446654,-3.96293892742527));
#19367=CARTESIAN_POINT('Ctrl Pts',(3.83471893698654,2.10385949889893,-3.9671560328369));
#19368=CARTESIAN_POINT('Ctrl Pts',(3.90592649960958,2.1433250527735,-3.97137313824853));
#19369=CARTESIAN_POINT('Ctrl Pts',(3.97713249661538,2.18278973893191,-3.97559015094005));
#19370=CARTESIAN_POINT('Ctrl Pts',(4.05030715930537,2.21870214556278,-3.97980716363158));
#19371=CARTESIAN_POINT('Ctrl Pts',(4.12505905264289,2.25087507715943,-3.9840241763231));
#19372=CARTESIAN_POINT('Ctrl Pts',(4.20012003786161,2.28318104073035,-3.98825862595605));
#19373=CARTESIAN_POINT('Ctrl Pts',(4.27677089659107,2.31171634042401,-3.992493075589));
#19374=CARTESIAN_POINT('Ctrl Pts',(4.35459609502854,2.33634066208324,-3.99672752522195));
#19375=CARTESIAN_POINT('Ctrl Pts',(4.43221317760941,2.36089913473858,-4.00095065132307));
#19376=CARTESIAN_POINT('Ctrl Pts',(4.51099786449122,2.38156744087855,-4.00517377742418));
#19377=CARTESIAN_POINT('Ctrl Pts',(4.59052558621481,2.39825723816322,-4.00939690352529));
#19378=CARTESIAN_POINT('Ctrl Pts',(4.67037316626169,2.41501416135643,-4.01363701492416));
#19379=CARTESIAN_POINT('Ctrl Pts',(4.7509693036795,2.42776044027575,-4.01787712632303));
#19380=CARTESIAN_POINT('Ctrl Pts',(4.83187878361868,2.43645917275322,-4.0221172377219));
#19381=CARTESIAN_POINT('Ctrl Pts',(4.91278826355786,2.44515790523068,-4.02635734912078));
#19382=CARTESIAN_POINT('Ctrl Pts',(4.99401061591388,2.4498091266479,-4.03059746051965));
#19383=CARTESIAN_POINT('Ctrl Pts',(5.07511218746176,2.45042853394525,-4.03483757191852));
#19384=CARTESIAN_POINT('Ctrl Pts',(5.15606115943214,2.45104677577454,-4.03906970518336));
#19385=CARTESIAN_POINT('Ctrl Pts',(5.23719177755503,2.44765068438233,-4.0433018384482));
#19386=CARTESIAN_POINT('Ctrl Pts',(5.3180731298665,2.44021802160368,-4.04753397171304));
#19387=CARTESIAN_POINT('Ctrl Pts',(5.39883889022776,2.43279598124864,-4.0517600566055));
#19388=CARTESIAN_POINT('Ctrl Pts',(5.47935563344585,2.42134886931261,-4.05598614149796));
#19389=CARTESIAN_POINT('Ctrl Pts',(5.55919194146204,2.40590645411306,-4.06021222639042));
#19390=CARTESIAN_POINT('Ctrl Pts',(5.6390491728845,2.39045999178338,-4.06443941885027));
#19391=CARTESIAN_POINT('Ctrl Pts',(5.71822514618863,2.37101615488072,-4.06866661131011));
#19392=CARTESIAN_POINT('Ctrl Pts',(5.79629272765714,2.34765678280878,-4.07289380376996));
#19393=CARTESIAN_POINT('Ctrl Pts',(5.8742002062599,2.32434531669652,-4.07711232700227));
#19394=CARTESIAN_POINT('Ctrl Pts',(5.95100338236365,2.29713446878585,-4.08133085023458));
#19395=CARTESIAN_POINT('Ctrl Pts',(6.02628923398334,2.26615637635691,-4.08554937346689));
#19396=CARTESIAN_POINT('Ctrl Pts',(6.10155039873976,2.23518844190474,-4.08976651340999));
#19397=CARTESIAN_POINT('Ctrl Pts',(6.17529479769941,2.20045589283366,-4.09398365335309));
#19398=CARTESIAN_POINT('Ctrl Pts',(6.24712797868544,2.16213955634959,-4.09820079329619));
#19399=CARTESIAN_POINT('Ctrl Pts',(6.31895958312151,2.12382406080865,-4.10241784068413));
#19400=CARTESIAN_POINT('Ctrl Pts',(6.38887964352791,2.08192515395072,-4.10663488807207));
#19401=CARTESIAN_POINT('Ctrl Pts',(6.45651825550695,2.03666963836407,-4.11085193546));
#19402=CARTESIAN_POINT('Ctrl Pts',(6.52443533872885,1.99122780376078,-4.1150863446239));
#19403=CARTESIAN_POINT('Ctrl Pts',(6.59005174893046,1.94240191503448,-4.11932075378779));
#19404=CARTESIAN_POINT('Ctrl Pts',(6.6530238504446,1.89046447105668,-4.12355516295168));
#19405=CARTESIAN_POINT('Ctrl Pts',(6.71582867230475,1.83866499416985,-4.12777832379318));
#19406=CARTESIAN_POINT('Ctrl Pts',(6.77600289862874,1.78377081761753,-4.13200148463468));
#19407=CARTESIAN_POINT('Ctrl Pts',(6.83324158643299,1.72609028943997,-4.13622464547618));
#19408=CARTESIAN_POINT('Ctrl Pts',(6.8907089557526,1.66817931449472,-4.14046467880127));
#19409=CARTESIAN_POINT('Ctrl Pts',(6.94521697288551,1.60746003379095,-4.14470471212637));
#19410=CARTESIAN_POINT('Ctrl Pts',(6.99649810553022,1.54427766471339,-4.14894474545146));
#19411=CARTESIAN_POINT('Ctrl Pts',(7.04777923817494,1.48109529563584,-4.15318477877655));
#19412=CARTESIAN_POINT('Ctrl Pts',(7.09583326051984,1.41545025193801,-4.15742481210164));
#19413=CARTESIAN_POINT('Ctrl Pts',(7.14043763352947,1.3477150296068,-4.16166484542674));
#19414=CARTESIAN_POINT('Ctrl Pts',(7.18580626204348,1.27881922563271,-4.1659775278799));
#19415=CARTESIAN_POINT('Ctrl Pts',(7.22777065721584,1.20751131754,-4.17029021033307));
#19416=CARTESIAN_POINT('Ctrl Pts',(7.26607126314968,1.13415421639984,-4.17460289278624));
#19417=CARTESIAN_POINT('Ctrl Pts',(7.3043109779799,1.06091373991189,-4.17890871884673));
#19418=CARTESIAN_POINT('Ctrl Pts',(7.33889827743594,0.985630932960405,-4.18321454490722));
#19419=CARTESIAN_POINT('Ctrl Pts',(7.36961702068705,0.908697275938748,-4.18752037096771));
#19420=CARTESIAN_POINT('Ctrl Pts',(7.40028604549749,0.831888136428436,-4.19181922802703));
#19421=CARTESIAN_POINT('Ctrl Pts',(7.42709881131217,0.753433871284795,-4.19611808508636));
#19422=CARTESIAN_POINT('Ctrl Pts',(7.44988591003959,0.673748762474872,-4.20041694214568));
#19423=CARTESIAN_POINT('Ctrl Pts',(7.47265125497041,0.594139725378565,-4.20471169528361));
#19424=CARTESIAN_POINT('Ctrl Pts',(7.49139844954934,0.513302602208026,-4.20900644842154));
#19425=CARTESIAN_POINT('Ctrl Pts',(7.50600706974429,0.431669214897464,-4.21330120155947));
#19426=CARTESIAN_POINT('Ctrl Pts',(7.52060499624227,0.350095584271307,-4.21759281088313));
#19427=CARTESIAN_POINT('Ctrl Pts',(7.53107029486122,0.267727281947792,-4.22188442020678));
#19428=CARTESIAN_POINT('Ctrl Pts',(7.53733333112178,0.185007620029785,-4.22617602953044));
#19429=CARTESIAN_POINT('Ctrl Pts',(7.54201981975292,0.123110364605593,-4.22938734389426));
#19430=CARTESIAN_POINT('Ctrl Pts',(7.54435442092451,0.0610166722415663,
-4.23259865825807));
#19431=CARTESIAN_POINT('Ctrl Pts',(7.54432691509289,-0.00108535955790657,
-4.23580997262189));
#19432=CARTESIAN_POINT('Ctrl Pts',(7.54432691509248,-0.00108536048783975,
-4.23580997266998));
#19433=CARTESIAN_POINT('Ctrl Pts',(7.54428737107733,-0.0903668487108589,
-4.24042674473442));
#19434=CARTESIAN_POINT('Ctrl Pts',(7.539364321265,-0.179489948314284,-4.24504351679887));
#19435=CARTESIAN_POINT('Ctrl Pts',(7.52963449131211,-0.267941920153354,
-4.24966028886331));
#19436=CARTESIAN_POINT('Ctrl Pts',(7.5198755875487,-0.35665819628985,-4.25429085635449));
#19437=CARTESIAN_POINT('Ctrl Pts',(7.50528126099808,-0.44469903253678,-4.25892142384567));
#19438=CARTESIAN_POINT('Ctrl Pts',(7.4859791683996,-0.531562787407136,-4.26355199133684));
#19439=CARTESIAN_POINT('Ctrl Pts',(7.46659045105702,-0.618816373095013,
-4.26820334008383));
#19440=CARTESIAN_POINT('Ctrl Pts',(7.44245175280597,-0.704882000402029,
-4.27285468883082));
#19441=CARTESIAN_POINT('Ctrl Pts',(7.41374111740686,-0.789271473659132,
-4.27750603757781));
#19442=CARTESIAN_POINT('Ctrl Pts',(7.39113710915984,-0.855711673360351,
-4.28116806469686));
#19443=CARTESIAN_POINT('Ctrl Pts',(7.3657001849672,-0.921113270048054,-4.28483009181591));
#19444=CARTESIAN_POINT('Ctrl Pts',(7.33753740143156,-0.98524848748491,-4.28849211893496));
#19445=CARTESIAN_POINT('Ctrl Pts',(7.30498972995338,-1.05936942743657,-4.29272431620567));
#19446=CARTESIAN_POINT('Ctrl Pts',(7.26870453158392,-1.13201406130332,-4.29695651347637));
#19447=CARTESIAN_POINT('Ctrl Pts',(7.22883777657832,-1.20278007037137,-4.30118871074708));
#19448=CARTESIAN_POINT('Ctrl Pts',(7.18902800658851,-1.27344492743585,-4.30541485857062));
#19449=CARTESIAN_POINT('Ctrl Pts',(7.14564707388499,-1.3422360915104,-4.30964100639415));
#19450=CARTESIAN_POINT('Ctrl Pts',(7.09889861254965,-1.40877205464076,-4.31386715421769));
#19451=CARTESIAN_POINT('Ctrl Pts',(7.05213877125819,-1.47532421458958,-4.31809433081042));
#19452=CARTESIAN_POINT('Ctrl Pts',(7.00200997354623,-1.53961965964256,-4.32232150740315));
#19453=CARTESIAN_POINT('Ctrl Pts',(6.94876160275957,-1.60130210959577,-4.32654868399587));
#19454=CARTESIAN_POINT('Ctrl Pts',(6.89562148097813,-1.6628591648421,-4.33076726713017));
#19455=CARTESIAN_POINT('Ctrl Pts',(6.83937474176338,-1.72181347026048,-4.33498585026446));
#19456=CARTESIAN_POINT('Ctrl Pts',(6.78031090742075,-1.77784217644569,-4.33920443339876));
#19457=CARTESIAN_POINT('Ctrl Pts',(6.72126645803511,-1.83385249381359,-4.34342163197932));
#19458=CARTESIAN_POINT('Ctrl Pts',(6.65940708651111,-1.88693879926115,-4.34763883055987));
#19459=CARTESIAN_POINT('Ctrl Pts',(6.59505915027523,-1.93681510416519,-4.35185602914043));
#19460=CARTESIAN_POINT('Ctrl Pts',(6.53071264666796,-1.9866902986339,-4.35607313383019));
#19461=CARTESIAN_POINT('Ctrl Pts',(6.4638780564703,-2.03335535089688,-4.36029023851994));
#19462=CARTESIAN_POINT('Ctrl Pts',(6.39491365015738,-2.07656547772955,-4.3645073432097));
#19463=CARTESIAN_POINT('Ctrl Pts',(6.32566742818896,-2.1199521781147,-4.36874168064582));
#19464=CARTESIAN_POINT('Ctrl Pts',(6.2542743400458,-2.15985539631951,-4.37297601808194));
#19465=CARTESIAN_POINT('Ctrl Pts',(6.18112357533096,-2.19607302823035,-4.37721035551806));
#19466=CARTESIAN_POINT('Ctrl Pts',(6.10816496908693,-2.23219552067421,-4.38143356984686));
#19467=CARTESIAN_POINT('Ctrl Pts',(6.03345835416626,-2.26465161685163,-4.38565678417567));
#19468=CARTESIAN_POINT('Ctrl Pts',(5.95740984230358,-2.29328916470909,-4.38987999850447));
#19469=CARTESIAN_POINT('Ctrl Pts',(5.88106088543859,-2.32203985098204,-4.39411989749425));
#19470=CARTESIAN_POINT('Ctrl Pts',(5.80335985837994,-2.34694161948083,-4.39835979648404));
#19471=CARTESIAN_POINT('Ctrl Pts',(5.72473115985107,-2.3678915488752,-4.40259969547382));
#19472=CARTESIAN_POINT('Ctrl Pts',(5.64610246132221,-2.38884147826957,-4.4068395944636));
#19473=CARTESIAN_POINT('Ctrl Pts',(5.56654656112702,-2.40583953172261,-4.41107949345339));
#19474=CARTESIAN_POINT('Ctrl Pts',(5.48649434772001,-2.41883499356968,-4.41531939244317));
#19475=CARTESIAN_POINT('Ctrl Pts',(5.40658499139273,-2.43180726438117,-4.41955172512639));
#19476=CARTESIAN_POINT('Ctrl Pts',(5.32588318725199,-2.4408395937733,-4.42378405780961));
#19477=CARTESIAN_POINT('Ctrl Pts',(5.24481144096651,-2.44584422961235,-4.42801639049282));
#19478=CARTESIAN_POINT('Ctrl Pts',(5.16385551824722,-2.45084171555273,-4.43224267663224));
#19479=CARTESIAN_POINT('Ctrl Pts',(5.08253116295906,-2.45182290803043,-4.43646896277166));
#19480=CARTESIAN_POINT('Ctrl Pts',(5.00126931782718,-2.44875137502647,-4.44069524891108));
#19481=CARTESIAN_POINT('Ctrl Pts',(4.91999100920527,-2.44567921973595,-4.44492239128776));
#19482=CARTESIAN_POINT('Ctrl Pts',(4.83877570024038,-2.43855264889365,-4.44914953366444));
#19483=CARTESIAN_POINT('Ctrl Pts',(4.75805796902285,-2.42738734104056,-4.45337667604112));
#19484=CARTESIAN_POINT('Ctrl Pts',(4.67750092251725,-2.41624425995536,-4.45759540344943));
#19485=CARTESIAN_POINT('Ctrl Pts',(4.59743993829805,-2.40107854452902,-4.46181413085774));
#19486=CARTESIAN_POINT('Ctrl Pts',(4.5183034039012,-2.3819577371145,-4.46603285826605));
#19487=CARTESIAN_POINT('Ctrl Pts',(4.43919280575068,-2.36284319636271,-4.47025020302658));
#19488=CARTESIAN_POINT('Ctrl Pts',(4.3610065070123,-2.33977624689354,-4.47446754778712));
#19489=CARTESIAN_POINT('Ctrl Pts',(4.28416197600715,-2.31287538514135,-4.47868489254765));
#19490=CARTESIAN_POINT('Ctrl Pts',(4.20731912492323,-2.28597511147693,-4.48290214511155));
#19491=CARTESIAN_POINT('Ctrl Pts',(4.13181842140342,-2.25524124677705,-4.48711939767545));
#19492=CARTESIAN_POINT('Ctrl Pts',(4.05806009290624,-2.22084147163705,-4.49133665023935));
#19493=CARTESIAN_POINT('Ctrl Pts',(3.98400591954238,-2.18630371890053,-4.49557081821536));
#19494=CARTESIAN_POINT('Ctrl Pts',(3.91170855971481,-2.14807077559741,-4.49980498619136));
#19495=CARTESIAN_POINT('Ctrl Pts',(3.84154913832487,-2.10635942275229,-4.50403915416736));
#19496=CARTESIAN_POINT('Ctrl Pts',(3.77156872390866,-2.06475449357623,-4.50826251895285));
#19497=CARTESIAN_POINT('Ctrl Pts',(3.70371571876488,-2.01968917518783,-4.51248588373834));
#19498=CARTESIAN_POINT('Ctrl Pts',(3.63833860513962,-1.97142165198274,-4.51670924852383));
#19499=CARTESIAN_POINT('Ctrl Pts',(3.57271064363016,-1.92296892931868,-4.52094881809509));
#19500=CARTESIAN_POINT('Ctrl Pts',(3.50957796964361,-1.87128968515863,-4.52518838766635));
#19501=CARTESIAN_POINT('Ctrl Pts',(3.44925757793471,-1.81668410977279,-4.52942795723761));
#19502=CARTESIAN_POINT('Ctrl Pts',(3.38893718622581,-1.76207853438695,-4.53366752680887));
#19503=CARTESIAN_POINT('Ctrl Pts',(3.33142936290843,-1.70454700184035,-4.53790709638013));
#19504=CARTESIAN_POINT('Ctrl Pts',(3.27701083001953,-1.64442351285733,-4.54214666595139));
#19505=CARTESIAN_POINT('Ctrl Pts',(3.22269977497076,-1.58441876913247,-4.54637786227633));
#19506=CARTESIAN_POINT('Ctrl Pts',(3.17126305689973,-1.52160829688815,-4.55060905860126));
#19507=CARTESIAN_POINT('Ctrl Pts',(3.12300395699217,-1.45629879159744,-4.5548402549262));
#19508=CARTESIAN_POINT('Ctrl Pts',(3.07481386315022,-1.3910826728808,-4.55906540103031));
#19509=CARTESIAN_POINT('Ctrl Pts',(3.02979263726867,-1.32337498893158,-4.56329054713442));
#19510=CARTESIAN_POINT('Ctrl Pts',(2.98820508344839,-1.25351742703743,-4.56751569323853));
#19511=CARTESIAN_POINT('Ctrl Pts',(2.94659507980136,-1.18362215457803,-4.5717431201644));
#19512=CARTESIAN_POINT('Ctrl Pts',(2.90842275172535,-1.11157504490533,-4.57597054709028));
#19513=CARTESIAN_POINT('Ctrl Pts',(2.873911367295,-1.03774955720847,-4.58019797401616));
#19514=CARTESIAN_POINT('Ctrl Pts',(2.83948031483959,-0.9640959127258,-4.58441556078177));
#19515=CARTESIAN_POINT('Ctrl Pts',(2.80869339990547,-0.88867257172208,-4.58863314754738));
#19516=CARTESIAN_POINT('Ctrl Pts',(2.78172676412774,-0.811875624977789,
-4.59285073431299));
#19517=CARTESIAN_POINT('Ctrl Pts',(2.75476895412816,-0.735103812730058,
-4.59706694072529));
#19518=CARTESIAN_POINT('Ctrl Pts',(2.73162909420773,-0.656959725825265,
-4.60128314713759));
#19519=CARTESIAN_POINT('Ctrl Pts',(2.71243462366512,-0.577857992541767,
-4.60549935354988));
#19520=CARTESIAN_POINT('Ctrl Pts',(2.69324055545416,-0.498757917294607,
-4.60971547158708));
#19521=CARTESIAN_POINT('Ctrl Pts',(2.6779918207041,-0.418700687646197,-4.61393158962428));
#19522=CARTESIAN_POINT('Ctrl Pts',(2.66676520413243,-0.338113197688939,
-4.61814770766147));
#19523=CARTESIAN_POINT('Ctrl Pts',(2.65548692612198,-0.257154868872812,
-4.62238322697798));
#19524=CARTESIAN_POINT('Ctrl Pts',(2.64826795247294,-0.17566185414372,-4.6266187462945));
#19525=CARTESIAN_POINT('Ctrl Pts',(2.64513349959239,-0.0940724707205781,
-4.63085426561101));
#19526=CARTESIAN_POINT('Ctrl Pts',(2.64200886573112,-0.0127386750374495,
-4.63507651669623));
#19527=CARTESIAN_POINT('Ctrl Pts',(2.64294315023596,0.0686904189995033,
-4.63929876778145));
#19528=CARTESIAN_POINT('Ctrl Pts',(2.64790901419109,0.14978216264069,-4.64352101886667));
#19529=CARTESIAN_POINT('Ctrl Pts',(2.65289828564739,0.231256146935658,-4.64776317229883));
#19530=CARTESIAN_POINT('Ctrl Pts',(2.66195718106376,0.312389122891401,-4.65200532573098));
#19531=CARTESIAN_POINT('Ctrl Pts',(2.67500575817194,0.392750936414906,-4.65624747916314));
#19532=CARTESIAN_POINT('Ctrl Pts',(2.68805433528013,0.473112749938412,-4.66048963259529));
#19533=CARTESIAN_POINT('Ctrl Pts',(2.70509243458295,0.55270295544313,-4.66473178602745));
#19534=CARTESIAN_POINT('Ctrl Pts',(2.7259896763458,0.631106902620107,-4.6689739394596));
#19535=CARTESIAN_POINT('Ctrl Pts',(2.74684211988583,0.709342772232802,-4.6732069988239));
#19536=CARTESIAN_POINT('Ctrl Pts',(2.77161505289539,0.786689742421022,-4.67744005818819));
#19537=CARTESIAN_POINT('Ctrl Pts',(2.80021567526547,0.862726276377071,-4.68167311755248));
#19538=CARTESIAN_POINT('Ctrl Pts',(2.82877539968435,0.938654080585398,-4.68590012378083));
#19539=CARTESIAN_POINT('Ctrl Pts',(2.8611517802724,1.01327473923382,-4.69012713000918));
#19540=CARTESIAN_POINT('Ctrl Pts',(2.89720173634656,1.08618001184655,-4.69435413623753));
#19541=CARTESIAN_POINT('Ctrl Pts',(2.9332513112152,1.15908451353207,-4.69858109776796));
#19542=CARTESIAN_POINT('Ctrl Pts',(2.97297423605483,1.23027322347637,-4.70280805929839));
#19543=CARTESIAN_POINT('Ctrl Pts',(3.01617851871151,1.29935614526803,-4.70703502082882));
#19544=CARTESIAN_POINT('Ctrl Pts',(3.05930578486468,1.36831591896504,-4.71125444732389));
#19545=CARTESIAN_POINT('Ctrl Pts',(3.10590178478073,1.43517699764488,-4.71547387381895));
#19546=CARTESIAN_POINT('Ctrl Pts',(3.15572961509238,1.49957599809002,-4.71969330031402));
#19547=CARTESIAN_POINT('Ctrl Pts',(3.20554100646591,1.56395375235252,-4.72391133475789));
#19548=CARTESIAN_POINT('Ctrl Pts',(3.25858182676458,1.62587067445297,-4.72812936920175));
#19549=CARTESIAN_POINT('Ctrl Pts',(3.31457314015658,1.68499418368467,-4.73234740364562));
#19550=CARTESIAN_POINT('Ctrl Pts',(3.37056309323716,1.74411625650811,-4.73656533561215));
#19551=CARTESIAN_POINT('Ctrl Pts',(3.42950307669267,1.80044471494321,-4.74078326757868));
#19552=CARTESIAN_POINT('Ctrl Pts',(3.49107632108868,1.85368282425665,-4.74500119954521));
#19553=CARTESIAN_POINT('Ctrl Pts',(3.5528744105041,1.90711534144708,-4.7492345339971));
#19554=CARTESIAN_POINT('Ctrl Pts',(3.61732467862498,1.95743458243436,-4.75346786844898));
#19555=CARTESIAN_POINT('Ctrl Pts',(3.68407373946097,2.00438158944311,-4.75770120290087));
#19556=CARTESIAN_POINT('Ctrl Pts',(3.75067581467381,2.05122521619462,-4.76192521528448));
#19557=CARTESIAN_POINT('Ctrl Pts',(3.81956615421436,2.09471122721534,-4.76614922766808));
#19558=CARTESIAN_POINT('Ctrl Pts',(3.89036656291258,2.13462709909764,-4.77037324005169));
#19559=CARTESIAN_POINT('Ctrl Pts',(3.96140134814094,2.17467510783792,-4.77461123553771));
#19560=CARTESIAN_POINT('Ctrl Pts',(4.03435844437011,2.21112910154888,-4.77884923102374));
#19561=CARTESIAN_POINT('Ctrl Pts',(4.10883482557177,2.24382271137337,-4.78308722650976));
#19562=CARTESIAN_POINT('Ctrl Pts',(4.18331120677344,2.27651632119785,-4.78732522199578));
#19563=CARTESIAN_POINT('Ctrl Pts',(4.2593064159903,2.30544943910065,-4.7915632174818));
#19564=CARTESIAN_POINT('Ctrl Pts',(4.33640305275022,2.3305061636144,-4.79580121296782));
#19565=CARTESIAN_POINT('Ctrl Pts',(4.41341477979149,2.35553529211985,-4.80003454097392));
#19566=CARTESIAN_POINT('Ctrl Pts',(4.49181135896812,2.37678947487168,-4.80426786898002));
#19567=CARTESIAN_POINT('Ctrl Pts',(4.57118839547999,2.39411757785071,-4.80850119698611));
#19568=CARTESIAN_POINT('Ctrl Pts',(4.65045229706855,2.41142098333929,-4.81272849129203));
#19569=CARTESIAN_POINT('Ctrl Pts',(4.73069343056475,2.42480932489246,-4.81695578559795));
#19570=CARTESIAN_POINT('Ctrl Pts',(4.81149125040211,2.43418090673619,-4.82118307990387));
#19571=CARTESIAN_POINT('Ctrl Pts',(4.89228137968239,2.44355159656718,-4.82540997184438));
#19572=CARTESIAN_POINT('Ctrl Pts',(4.97362763800656,2.4489061761921,-4.82963686378488));
#19573=CARTESIAN_POINT('Ctrl Pts',(5.05509834107404,2.45019393700515,-4.83386375572539));
#19574=CARTESIAN_POINT('Ctrl Pts',(5.13643156187334,2.4514795247146,-4.83808351476205));
#19575=CARTESIAN_POINT('Ctrl Pts',(5.21788834432283,2.44871197281434,-4.84230327379871));
#19576=CARTESIAN_POINT('Ctrl Pts',(5.29903483032702,2.44189272085668,-4.84652303283537));
#19577=CARTESIAN_POINT('Ctrl Pts',(5.38015485222368,2.43507569284519,-4.85074141569221));
#19578=CARTESIAN_POINT('Ctrl Pts',(5.46096431626495,2.42420962781349,-4.85495979854904));
#19579=CARTESIAN_POINT('Ctrl Pts',(5.5410323879996,2.40934798856102,-4.85917818140588));
#19580=CARTESIAN_POINT('Ctrl Pts',(5.62109880477188,2.39448665649035,-4.86339647707109));
#19581=CARTESIAN_POINT('Ctrl Pts',(5.70042340335079,2.37563000029033,-4.86761477273631));
#19582=CARTESIAN_POINT('Ctrl Pts',(5.77858488702693,2.35288272105727,-4.87183306840152));
#19583=CARTESIAN_POINT('Ctrl Pts',(5.85701793115484,2.33005640978523,-4.87606601990773));
#19584=CARTESIAN_POINT('Ctrl Pts',(5.93427931019796,2.30331251641365,-4.88029897141394));
#19585=CARTESIAN_POINT('Ctrl Pts',(6.00995976488316,2.27280691919461,-4.88453192292015));
#19586=CARTESIAN_POINT('Ctrl Pts',(6.08548749420368,2.24236288316041,-4.88875633220677));
#19587=CARTESIAN_POINT('Ctrl Pts',(6.15944026498193,2.20817253964699,-4.89298074149339));
#19588=CARTESIAN_POINT('Ctrl Pts',(6.23143409427271,2.17043790575762,-4.89720515078002));
#19589=CARTESIAN_POINT('Ctrl Pts',(6.30364629270944,2.13258881650649,-4.90144237339602));
#19590=CARTESIAN_POINT('Ctrl Pts',(6.37388725118885,2.09117415365666,-4.90567959601202));
#19591=CARTESIAN_POINT('Ctrl Pts',(6.44179853445689,2.04644164622074,-4.90991681862802));
#19592=CARTESIAN_POINT('Ctrl Pts',(6.50970981772493,2.00170913878482,-4.91415404124403));
#19593=CARTESIAN_POINT('Ctrl Pts',(6.57529108735771,1.95365911117781,-4.91839126386003));
#19594=CARTESIAN_POINT('Ctrl Pts',(6.63821842469443,1.90257873884136,-4.92262848647603));
#19595=CARTESIAN_POINT('Ctrl Pts',(6.70017391982866,1.85228724560987,-4.92680026993739));
#19596=CARTESIAN_POINT('Ctrl Pts',(6.75980233382613,1.79885885488646,-4.93097205339874));
#19597=CARTESIAN_POINT('Ctrl Pts',(6.81676205169122,1.74253998327872,-4.9351438368601));
#19598=CARTESIAN_POINT('Ctrl Pts',(6.87403087073743,1.68591548814638,-4.93933825918351));
#19599=CARTESIAN_POINT('Ctrl Pts',(6.92860151443369,1.62636928924725,-4.94353268150691));
#19600=CARTESIAN_POINT('Ctrl Pts',(6.98015822822778,1.5641947877054,-4.94772710383032));
#19601=CARTESIAN_POINT('Ctrl Pts',(7.03130380679619,1.50251609215742,-4.95188807804112));
#19602=CARTESIAN_POINT('Ctrl Pts',(7.07948302343086,1.43825122094879,-4.95604905225193));
#19603=CARTESIAN_POINT('Ctrl Pts',(7.12442395388076,1.37172405833512,-4.96021002646273));
#19604=CARTESIAN_POINT('Ctrl Pts',(7.16933776961209,1.305237034305,-4.96436849018602));
#19605=CARTESIAN_POINT('Ctrl Pts',(7.21101690765184,1.23649082270111,-4.96852695390931));
#19606=CARTESIAN_POINT('Ctrl Pts',(7.24923098070076,1.16584072673234,-4.9726854176326));
#19607=CARTESIAN_POINT('Ctrl Pts',(7.28743447585925,1.09521018714463,-4.97684273026755));
#19608=CARTESIAN_POINT('Ctrl Pts',(7.32217458279344,1.0226772308401,-4.98100004290251));
#19609=CARTESIAN_POINT('Ctrl Pts',(7.35326619168597,0.948622944876998,-4.98515735553747));
#19610=CARTESIAN_POINT('Ctrl Pts',(7.3848344886857,0.873433278704817,-4.98937840696117));
#19611=CARTESIAN_POINT('Ctrl Pts',(7.41264123776607,0.79667569270143,-4.99359945838487));
#19612=CARTESIAN_POINT('Ctrl Pts',(7.43654358952192,0.718769754193858,-4.99782050980857));
#19613=CARTESIAN_POINT('Ctrl Pts',(7.46010728211529,0.64196762171163,-5.00198175549623));
#19614=CARTESIAN_POINT('Ctrl Pts',(7.47987644130325,0.564049955605879,-5.00614300118389));
#19615=CARTESIAN_POINT('Ctrl Pts',(7.4957652064418,0.485431611262245,-5.01030424687154));
#19616=CARTESIAN_POINT('Ctrl Pts',(7.51199650337201,0.405118403780354,-5.01455520116327));
#19617=CARTESIAN_POINT('Ctrl Pts',(7.52417805709933,0.32407447512187,-5.01880615545499));
#19618=CARTESIAN_POINT('Ctrl Pts',(7.53227411923112,0.242748130459943,-5.02305710974672));
#19619=CARTESIAN_POINT('Ctrl Pts',(7.54037018136291,0.161421785798016,-5.02730806403844));
#19620=CARTESIAN_POINT('Ctrl Pts',(7.5443807895523,0.0798135539581412,-5.03155901833017));
#19621=CARTESIAN_POINT('Ctrl Pts',(7.54432661329192,-0.00163007106614652,
-5.03580997262189));
#19622=CARTESIAN_POINT('Origin',(5.09382715545311,0.,-6.77268258743872));
#19623=CARTESIAN_POINT('',(6.2322445509742,-1.63799676314545,12.7063625311661));
#19624=CARTESIAN_POINT('Ctrl Pts',(6.2322445509742,-1.63799676314545,12.7063625311661));
#19625=CARTESIAN_POINT('Ctrl Pts',(6.18723751963155,-1.66927691494676,12.7026454909915));
#19626=CARTESIAN_POINT('Ctrl Pts',(6.14095921641945,-1.69868960221159,12.6988580646124));
#19627=CARTESIAN_POINT('Ctrl Pts',(5.93503956423552,-1.81794739040668,12.6823136378186));
#19628=CARTESIAN_POINT('Ctrl Pts',(5.76462383730148,-1.88749318531041,12.6695051840078));
#19629=CARTESIAN_POINT('Ctrl Pts',(5.56341161226874,-1.93884377134319,12.6559190568223));
#19630=CARTESIAN_POINT('Ctrl Pts',(5.5396236298541,-1.94445116206349,12.6543338775543));
#19631=CARTESIAN_POINT('Ctrl Pts',(5.50499088329774,-1.95194591492976,12.6520553073756));
#19632=CARTESIAN_POINT('Ctrl Pts',(5.49422482639037,-1.95418273937355,12.651351047854));
#19633=CARTESIAN_POINT('Ctrl Pts',(5.47532410946914,-1.95794691645816,12.6501216010108));
#19634=CARTESIAN_POINT('Ctrl Pts',(5.46719749484511,-1.95951285950553,12.6495952228125));
#19635=CARTESIAN_POINT('Ctrl Pts',(5.45032734667706,-1.96265486105093,12.6485070419849));
#19636=CARTESIAN_POINT('Ctrl Pts',(5.44158254368898,-1.96422317569687,12.6479454902952));
#19637=CARTESIAN_POINT('Ctrl Pts',(5.41897191528525,-1.96812248926442,12.646499853696));
#19638=CARTESIAN_POINT('Ctrl Pts',(5.40509124865864,-1.97036542993468,12.6456184974278));
#19639=CARTESIAN_POINT('Ctrl Pts',(5.34912562121874,-1.97880258950332,12.6420882725356));
#19640=CARTESIAN_POINT('Ctrl Pts',(5.30686941728698,-1.98379695924688,12.6394760781965));
#19641=CARTESIAN_POINT('Ctrl Pts',(5.11806873338589,-2.00000880851574,12.6279896156928));
#19642=CARTESIAN_POINT('Ctrl Pts',(4.97071634581146,-1.99636377597456,12.6195567854678));
#19643=CARTESIAN_POINT('Ctrl Pts',(4.73572640100998,-1.96441495345043,12.6056334717768));
#19644=CARTESIAN_POINT('Ctrl Pts',(4.64729381143923,-1.94621841789028,12.600269460508));
#19645=CARTESIAN_POINT('Ctrl Pts',(4.54986226646271,-1.91917939090682,12.5939245573538));
#19646=CARTESIAN_POINT('Ctrl Pts',(4.5393412980253,-1.91616616098604,12.5932335632078));
#19647=CARTESIAN_POINT('Ctrl Pts',(4.52349276982025,-1.91148565433896,12.5921830685969));
#19648=CARTESIAN_POINT('Ctrl Pts',(4.518146344896,-1.90988227929641,12.5918270316851));
#19649=CARTESIAN_POINT('Ctrl Pts',(4.51277827934583,-1.90824782640071,12.59146781953));
#19650=CARTESIAN_POINT('Ctrl Pts',(4.51274976313558,-1.90823914316996,12.5914659112757));
#19651=CARTESIAN_POINT('Ctrl Pts',(4.51269202440837,-1.9082215602227,12.5914620474027));
#19652=CARTESIAN_POINT('Ctrl Pts',(4.51266280188701,-1.90821266046981,12.5914600917812));
#19653=CARTESIAN_POINT('Ctrl Pts',(4.51260362535662,-1.90819463670315,12.5914561314808));
#19654=CARTESIAN_POINT('Ctrl Pts',(4.51257367136493,-1.90818551265747,12.5914541268006));
#19655=CARTESIAN_POINT('Ctrl Pts',(4.51251300550165,-1.90816703215337,12.5914500666086));
#19656=CARTESIAN_POINT('Ctrl Pts',(4.51248229364932,-1.90815767566129,12.5914480110954));
#19657=CARTESIAN_POINT('Ctrl Pts',(4.51242008440394,-1.90813872171764,12.5914438473776));
#19658=CARTESIAN_POINT('Ctrl Pts',(4.5123885870135,-1.90812912422485,12.5914417391702));
#19659=CARTESIAN_POINT('Ctrl Pts',(4.51232477765905,-1.90810967930591,12.591437468112));
#19660=CARTESIAN_POINT('Ctrl Pts',(4.51229246569785,-1.90809983183592,12.5914353052581));
#19661=CARTESIAN_POINT('Ctrl Pts',(4.51222699669508,-1.90807987752981,12.5914309228552));
#19662=CARTESIAN_POINT('Ctrl Pts',(4.51219383968033,-1.90806977065429,12.5914287033046));
#19663=CARTESIAN_POINT('Ctrl Pts',(4.51212664853273,-1.90804928762717,12.5914242053533));
#19664=CARTESIAN_POINT('Ctrl Pts',(4.51209261441863,-1.90803891143063,12.5914219269504));
#19665=CARTESIAN_POINT('Ctrl Pts',(4.5120236354109,-1.90801787934526,12.5914173090301));
#19666=CARTESIAN_POINT('Ctrl Pts',(4.51198869051462,-1.90800722340161,12.5914149695088));
#19667=CARTESIAN_POINT('Ctrl Pts',(4.51191785450351,-1.90798562085157,12.5914102269676));
#19668=CARTESIAN_POINT('Ctrl Pts',(4.51188196341328,-1.90797467419506,12.5914078239452));
#19669=CARTESIAN_POINT('Ctrl Pts',(4.51180919772279,-1.90795247867071,12.5914029518929));
#19670=CARTESIAN_POINT('Ctrl Pts',(4.51177232313178,-1.90794122974416,12.5914004828591));
#19671=CARTESIAN_POINT('Ctrl Pts',(4.51169755113618,-1.90791841750315,12.5913954761388));
#19672=CARTESIAN_POINT('Ctrl Pts',(4.51165965378225,-1.90790685413838,12.5913929384511));
#19673=CARTESIAN_POINT('Ctrl Pts',(4.5115827948851,-1.9078834001967,12.5913877916382));
#19674=CARTESIAN_POINT('Ctrl Pts',(4.51154383333025,-1.9078715095459,12.5913851825073));
#19675=CARTESIAN_POINT('Ctrl Pts',(4.51146480235348,-1.90784738748869,12.591379889868));
#19676=CARTESIAN_POINT('Ctrl Pts',(4.51142473296251,-1.90783515601643,12.5913772063563));
#19677=CARTESIAN_POINT('Ctrl Pts',(4.51134344021335,-1.90781033801536,12.5913717618517));
#19678=CARTESIAN_POINT('Ctrl Pts',(4.51130221687445,-1.90779775141175,12.5913690008544));
#19679=CARTESIAN_POINT('Ctrl Pts',(4.50696216130483,-1.90647246093234,12.5910783079931));
#19680=CARTESIAN_POINT('Ctrl Pts',(4.5026679041137,-1.90514527129782,12.5907895540963));
#19681=CARTESIAN_POINT('Ctrl Pts',(4.49303084428502,-1.90213110618786,12.5901389583457));
#19682=CARTESIAN_POINT('Ctrl Pts',(4.48769074418875,-1.9004361609251,12.5897766755344));
#19683=CARTESIAN_POINT('Ctrl Pts',(4.47199469809999,-1.89538135804588,12.5887067416442));
#19684=CARTESIAN_POINT('Ctrl Pts',(4.46165923216744,-1.89195924946562,12.5879956852284));
#19685=CARTESIAN_POINT('Ctrl Pts',(4.36404925557136,-1.85875114981835,12.5812216900391));
#19686=CARTESIAN_POINT('Ctrl Pts',(4.27892038465484,-1.82303445481991,12.5748729694351));
#19687=CARTESIAN_POINT('Ctrl Pts',(4.07991571698058,-1.72280969877737,12.5593908680569));
#19688=CARTESIAN_POINT('Ctrl Pts',(3.96929305990238,-1.65273095111793,12.5502534644303));
#19689=CARTESIAN_POINT('Ctrl Pts',(3.81805608485066,-1.53466072923676,12.53732382093));
#19690=CARTESIAN_POINT('Ctrl Pts',(3.77155685309105,-1.49478357640746,12.5332730538595));
#19691=CARTESIAN_POINT('Ctrl Pts',(3.71588647170828,-1.44240710531632,12.5283236466226));
#19692=CARTESIAN_POINT('Ctrl Pts',(3.70493080994919,-1.43186093873175,12.5273444003053));
#19693=CARTESIAN_POINT('Ctrl Pts',(3.68763813144638,-1.41482937616726,12.5257899741617));
#19694=CARTESIAN_POINT('Ctrl Pts',(3.68122305381124,-1.4084244358007,12.5252113539758));
#19695=CARTESIAN_POINT('Ctrl Pts',(3.66916162512141,-1.39621675777233,12.524119583994));
#19696=CARTESIAN_POINT('Ctrl Pts',(3.66350652545945,-1.39042295958586,12.5236060583568));
#19697=CARTESIAN_POINT('Ctrl Pts',(3.65075984945893,-1.37720359293777,12.5224447172042));
#19698=CARTESIAN_POINT('Ctrl Pts',(3.6436899808946,-1.36975733883143,12.5217978416863));
#19699=CARTESIAN_POINT('Ctrl Pts',(3.62555380862095,-1.35035782979332,12.520130996751));
#19700=CARTESIAN_POINT('Ctrl Pts',(3.61457572156844,-1.33832287180318,12.5191147470155));
#19701=CARTESIAN_POINT('Ctrl Pts',(3.51656816852848,-1.2282005562993,12.5099708012622));
#19702=CARTESIAN_POINT('Ctrl Pts',(3.43925665749271,-1.1218848075501,12.5022693904214));
#19703=CARTESIAN_POINT('Ctrl Pts',(3.32540327515749,-0.927651995339202,
12.4891855523885));
#19704=CARTESIAN_POINT('Ctrl Pts',(3.28366670373308,-0.843314085038435,
12.4837723108124));
#19705=CARTESIAN_POINT('Ctrl Pts',(3.23300736711884,-0.719685733890782,
12.4758239730855));
#19706=CARTESIAN_POINT('Ctrl Pts',(3.21907889568554,-0.682580702392783,
12.4734360065092));
#19707=CARTESIAN_POINT('Ctrl Pts',(3.19860980746405,-0.622687060603674,
12.4695414513147));
#19708=CARTESIAN_POINT('Ctrl Pts',(3.19135390953321,-0.600152817296067,
12.4680673079187));
#19709=CARTESIAN_POINT('Ctrl Pts',(3.18231918289361,-0.570282065938907,
12.4660950865986));
#19710=CARTESIAN_POINT('Ctrl Pts',(3.18017820016021,-0.563055978985791,
12.4656165954773));
#19711=CARTESIAN_POINT('Ctrl Pts',(3.17673380241601,-0.551184106655632,
12.4648279389091));
#19712=CARTESIAN_POINT('Ctrl Pts',(3.1754061811022,-0.546545339072591,12.464519150038));
#19713=CARTESIAN_POINT('Ctrl Pts',(3.17285136171797,-0.537494682097194,
12.4639153617674));
#19714=CARTESIAN_POINT('Ctrl Pts',(3.17162251456136,-0.533083342655446,
12.4636204581332));
#19715=CARTESIAN_POINT('Ctrl Pts',(3.16863876911263,-0.522227773975677,
12.4628932957496));
#19716=CARTESIAN_POINT('Ctrl Pts',(3.16690103708571,-0.515778927514173,
12.4624600653469));
#19717=CARTESIAN_POINT('Ctrl Pts',(3.16105405416527,-0.493638348530498,
12.4609686707115));
#19718=CARTESIAN_POINT('Ctrl Pts',(3.15710396446798,-0.477905766142753,
12.4599020482814));
#19719=CARTESIAN_POINT('Ctrl Pts',(3.13039713457844,-0.365763327402304,
12.4522588648364));
#19720=CARTESIAN_POINT('Ctrl Pts',(3.11466022664813,-0.26783309454235,12.4453805421707));
#19721=CARTESIAN_POINT('Ctrl Pts',(3.09619549174484,-0.0508676684509539,
12.4301977354646));
#19722=CARTESIAN_POINT('Ctrl Pts',(3.09670693678055,0.0680909993364611,
12.4219194855569));
#19723=CARTESIAN_POINT('Ctrl Pts',(3.11338612636969,0.245891031721891,12.4098909324857));
#19724=CARTESIAN_POINT('Ctrl Pts',(3.12165462170422,0.305197996803086,12.4059332340362));
#19725=CARTESIAN_POINT('Ctrl Pts',(3.13531309294309,0.378780583618809,12.401089088398));
#19726=CARTESIAN_POINT('Ctrl Pts',(3.13821356534267,0.393481346636533,12.4001245546047));
#19727=CARTESIAN_POINT('Ctrl Pts',(3.14310968073674,0.416903953167463,12.3985926660017));
#19728=CARTESIAN_POINT('Ctrl Pts',(3.14499878804879,0.425647237797762,12.3980219300497));
#19729=CARTESIAN_POINT('Ctrl Pts',(3.14868775248628,0.44218117563066,12.396944614798));
#19730=CARTESIAN_POINT('Ctrl Pts',(3.15047575830151,0.449974265149608,12.396437667005));
#19731=CARTESIAN_POINT('Ctrl Pts',(3.15463928449656,0.467633337781124,12.3952907195161));
#19732=CARTESIAN_POINT('Ctrl Pts',(3.15704334351841,0.477492418203566,12.3946516515278));
#19733=CARTESIAN_POINT('Ctrl Pts',(3.16345856869421,0.502955505473551,12.3930041633034));
#19734=CARTESIAN_POINT('Ctrl Pts',(3.16758377758906,0.518530225055481,12.3919994293147));
#19735=CARTESIAN_POINT('Ctrl Pts',(3.20654119372476,0.658728544150087,12.3829776374736));
#19736=CARTESIAN_POINT('Ctrl Pts',(3.25323521727404,0.779743135453562,12.3753793957891));
#19737=CARTESIAN_POINT('Ctrl Pts',(3.35289618582782,0.978141931426943,12.3624883358535));
#19738=CARTESIAN_POINT('Ctrl Pts',(3.40017137634611,1.0578897922908,12.3571622729389));
#19739=CARTESIAN_POINT('Ctrl Pts',(3.48778134483719,1.18466360433034,12.3480200883196));
#19740=CARTESIAN_POINT('Ctrl Pts',(3.52506920610242,1.23361577413524,12.3443007546343));
#19741=CARTESIAN_POINT('Ctrl Pts',(3.57096387177269,1.28841555581908,12.3398099546415));
#19742=CARTESIAN_POINT('Ctrl Pts',(3.57743090723702,1.29602069188735,12.3391790086005));
#19743=CARTESIAN_POINT('Ctrl Pts',(3.58743845899392,1.30761197525262,12.3382048798982));
#19744=CARTESIAN_POINT('Ctrl Pts',(3.59093843681843,1.31163313485098,12.3378646075071));
#19745=CARTESIAN_POINT('Ctrl Pts',(3.59741173006245,1.31901044025377,12.3372359172888));
#19746=CARTESIAN_POINT('Ctrl Pts',(3.60038028502556,1.32237064037352,12.3369478499126));
#19747=CARTESIAN_POINT('Ctrl Pts',(3.6071076499983,1.32993400961694,12.3362955972534));
#19748=CARTESIAN_POINT('Ctrl Pts',(3.61087297425112,1.33413127255403,12.3359309324031));
#19749=CARTESIAN_POINT('Ctrl Pts',(3.62060707019488,1.344889891772,12.3349893639296));
#19750=CARTESIAN_POINT('Ctrl Pts',(3.62660182826597,1.3514274205184,12.3344106091692));
#19751=CARTESIAN_POINT('Ctrl Pts',(3.66443928092342,1.39214220329821,12.3307657816568));
#19752=CARTESIAN_POINT('Ctrl Pts',(3.69742815539956,1.42522934092756,12.327624001904));
#19753=CARTESIAN_POINT('Ctrl Pts',(3.74617306669238,1.47080149990933,12.3230692513813));
#19754=CARTESIAN_POINT('Ctrl Pts',(3.76100628899616,1.48425641121027,12.3216940853168));
#19755=CARTESIAN_POINT('Ctrl Pts',(3.88677879421587,1.59493628545549,12.3101392768706));
#19756=CARTESIAN_POINT('Ctrl Pts',(4.00800176840245,1.67981488847997,12.299722688753));
#19757=CARTESIAN_POINT('Ctrl Pts',(4.2008405366079,1.78516543736933,12.2848115688193));
#19758=CARTESIAN_POINT('Ctrl Pts',(4.26604209303637,1.81631901648813,12.2800110676617));
#19759=CARTESIAN_POINT('Ctrl Pts',(4.34751462023686,1.84994558677418,12.2742990684326));
#19760=CARTESIAN_POINT('Ctrl Pts',(4.36230490152697,1.85584382168861,12.2732731313827));
#19761=CARTESIAN_POINT('Ctrl Pts',(4.38575737200205,1.86487252204341,12.271663242785));
#19762=CARTESIAN_POINT('Ctrl Pts',(4.39437308076907,1.86812107310452,12.2710753834234));
#19763=CARTESIAN_POINT('Ctrl Pts',(4.41056577820019,1.87409879784304,12.2699770900376));
#19764=CARTESIAN_POINT('Ctrl Pts',(4.41813737017176,1.876841956819,12.2694662022758));
#19765=CARTESIAN_POINT('Ctrl Pts',(4.43513750058359,1.88288482938028,12.2683249895967));
#19766=CARTESIAN_POINT('Ctrl Pts',(4.4445746745822,1.88615973979641,12.2676954906258));
#19767=CARTESIAN_POINT('Ctrl Pts',(4.46863667263551,1.89430780001674,12.2661003878841));
#19768=CARTESIAN_POINT('Ctrl Pts',(4.48329428160301,1.89908262370223,12.265137995578));
#19769=CARTESIAN_POINT('Ctrl Pts',(4.57630408552551,1.92819307903178,12.2590869040561));
#19770=CARTESIAN_POINT('Ctrl Pts',(4.65604460436796,1.94784687925749,12.2541525791783));
#19771=CARTESIAN_POINT('Ctrl Pts',(4.87062024860056,1.98688529734874,12.2412754013749));
#19772=CARTESIAN_POINT('Ctrl Pts',(5.00659553874558,1.99747901975286,12.2335393632787));
#19773=CARTESIAN_POINT('Ctrl Pts',(5.20669153551384,1.9925865806146,12.2216712890258));
#19774=CARTESIAN_POINT('Ctrl Pts',(5.27067835883385,1.98792895377555,12.2177979524977));
#19775=CARTESIAN_POINT('Ctrl Pts',(5.34441016464217,1.97897422467048,12.2131319487659));
#19776=CARTESIAN_POINT('Ctrl Pts',(5.3544881651005,1.97767202898286,12.2124897462396));
#19777=CARTESIAN_POINT('Ctrl Pts',(5.36991655704566,1.97555852478028,12.2114991972189));
#19778=CARTESIAN_POINT('Ctrl Pts',(5.37527450285379,1.97480232719358,12.211153829856));
#19779=CARTESIAN_POINT('Ctrl Pts',(5.38509282836015,1.97337584219566,12.2105183265323));
#19780=CARTESIAN_POINT('Ctrl Pts',(5.38955406899058,1.97271221883778,12.2102285642118));
#19781=CARTESIAN_POINT('Ctrl Pts',(5.3995884364275,1.97118477234887,12.2095745560146));
#19782=CARTESIAN_POINT('Ctrl Pts',(5.40516011362618,1.9703124510988,12.2092098486817));
#19783=CARTESIAN_POINT('Ctrl Pts',(5.42155091597614,1.96767499074004,12.2081324942697));
#19784=CARTESIAN_POINT('Ctrl Pts',(5.43235906903729,1.965844312991,12.207416360505));
#19785=CARTESIAN_POINT('Ctrl Pts',(5.53867668276732,1.94693355315497,12.200319058902));
#19786=CARTESIAN_POINT('Ctrl Pts',(5.63282436823093,1.9229973877585,12.1936192697975));
#19787=CARTESIAN_POINT('Ctrl Pts',(5.84595090681782,1.85192737131336,12.1779824887464));
#19788=CARTESIAN_POINT('Ctrl Pts',(5.96291472946638,1.80000517724095,12.1690571620422));
#19789=CARTESIAN_POINT('Ctrl Pts',(6.12688048745212,1.70748305145927,12.1563727763964));
#19790=CARTESIAN_POINT('Ctrl Pts',(6.17826131600852,1.6753212809606,12.1523654154912));
#19791=CARTESIAN_POINT('Ctrl Pts',(6.24053571284764,1.63227310121271,12.1474643296516));
#19792=CARTESIAN_POINT('Ctrl Pts',(6.25287049849402,1.62353766271917,12.1464912115559));
#19793=CARTESIAN_POINT('Ctrl Pts',(6.27240458806707,1.60936761433364,12.1449460107085));
#19794=CARTESIAN_POINT('Ctrl Pts',(6.27966818607189,1.60402304759612,12.1443705138342));
#19795=CARTESIAN_POINT('Ctrl Pts',(6.29335347991602,1.59380961724399,12.143284356848));
#19796=CARTESIAN_POINT('Ctrl Pts',(6.29978238016489,1.5889507538589,12.1427733245512));
#19797=CARTESIAN_POINT('Ctrl Pts',(6.31430179991397,1.57783831950005,12.1416172706325));
#19798=CARTESIAN_POINT('Ctrl Pts',(6.32237407443138,1.57156119650483,12.1409731868925));
#19799=CARTESIAN_POINT('Ctrl Pts',(6.34313511373106,1.55515937638821,12.1393128586219));
#19800=CARTESIAN_POINT('Ctrl Pts',(6.35574935547309,1.54494124349367,12.1383003251915));
#19801=CARTESIAN_POINT('Ctrl Pts',(6.46689292308435,1.45264011801318,12.1293409610452));
#19802=CARTESIAN_POINT('Ctrl Pts',(6.5574229852202,1.36138401169962,12.1218012028334));
#19803=CARTESIAN_POINT('Ctrl Pts',(6.69624716482366,1.1914642308639,12.109044984281));
#19804=CARTESIAN_POINT('Ctrl Pts',(6.74901103184418,1.11700573473798,12.1037947930387));
#19805=CARTESIAN_POINT('Ctrl Pts',(6.82926078749395,0.985521692073947,12.0946578200157));
#19806=CARTESIAN_POINT('Ctrl Pts',(6.85946477614059,0.930325206395275,12.0908566646311));
#19807=CARTESIAN_POINT('Ctrl Pts',(6.89142762493263,0.864732262928983,12.0862723767022));
#19808=CARTESIAN_POINT('Ctrl Pts',(6.89577779887109,0.855630295769165,12.0856347756757));
#19809=CARTESIAN_POINT('Ctrl Pts',(6.90234160229976,0.841624619315283,12.0846508354907));
#19810=CARTESIAN_POINT('Ctrl Pts',(6.90460481827666,0.836744141583591,12.0843074444435));
#19811=CARTESIAN_POINT('Ctrl Pts',(6.90872239383953,0.827769915867824,12.0836749510917));
#19812=CARTESIAN_POINT('Ctrl Pts',(6.91058268539381,0.8236790049598,12.0833862156832));
#19813=CARTESIAN_POINT('Ctrl Pts',(6.91474172076468,0.814450359628221,12.0827339330049));
#19814=CARTESIAN_POINT('Ctrl Pts',(6.91703253430751,0.809309203643577,12.0823699206554));
#19815=CARTESIAN_POINT('Ctrl Pts',(6.9237146727944,0.794140461947037,12.081294202982));
#19816=CARTESIAN_POINT('Ctrl Pts',(6.92804516097314,0.784086535218607,12.0805790113496));
#19817=CARTESIAN_POINT('Ctrl Pts',(6.97014991853022,0.684075727522825,12.0734465813574));
#19818=CARTESIAN_POINT('Ctrl Pts',(7.00135464276814,0.591507502141149,12.0667064368498));
#19819=CARTESIAN_POINT('Ctrl Pts',(7.05741340275238,0.373625754207483,12.051043138094));
#19820=CARTESIAN_POINT('Ctrl Pts',(7.07727084328638,0.247436917017078,12.0421331004315));
#19821=CARTESIAN_POINT('Ctrl Pts',(7.08736833456825,0.0801813959388592,
12.030843681731));
#19822=CARTESIAN_POINT('Ctrl Pts',(7.0885771551553,0.0400941634017856,12.0281742241702));
#19823=CARTESIAN_POINT('Ctrl Pts',(7.08857715545311,1.48164940157807E-8,
12.0255409243712));
#19824=CARTESIAN_POINT('',(3.93347817078409,-1.62253437445176,12.7063625311661));
#19825=CARTESIAN_POINT('Origin',(5.09382715545311,0.,12.7063625311661));
#19826=CARTESIAN_POINT('Ctrl Pts',(7.08857671409759,0.0013269467482341,
12.1854076497708));
#19827=CARTESIAN_POINT('Ctrl Pts',(7.08852952443368,0.0722654085738397,
12.1899562455583));
#19828=CARTESIAN_POINT('Ctrl Pts',(7.08469842768434,0.143085755684006,12.1945048413457));
#19829=CARTESIAN_POINT('Ctrl Pts',(7.07711961581017,0.213491403084141,12.1990534371332));
#19830=CARTESIAN_POINT('Ctrl Pts',(7.0696816549397,0.282588572814277,12.2035174979971));
#19831=CARTESIAN_POINT('Ctrl Pts',(7.05861405494534,0.351430098961739,12.2079815588611));
#19832=CARTESIAN_POINT('Ctrl Pts',(7.04394472965862,0.419605778409722,12.212445619725));
#19833=CARTESIAN_POINT('Ctrl Pts',(7.0292973878188,0.487679289802924,12.2169029907485));
#19834=CARTESIAN_POINT('Ctrl Pts',(7.01105913665847,0.555088462726542,12.2213603617721));
#19835=CARTESIAN_POINT('Ctrl Pts',(6.98930956850293,0.621428985740803,12.2258177327956));
#19836=CARTESIAN_POINT('Ctrl Pts',(6.96758580705325,0.687690793152414,12.2302698149756));
#19837=CARTESIAN_POINT('Ctrl Pts',(6.94235915592093,0.75288600875125,12.2347218971556));
#19838=CARTESIAN_POINT('Ctrl Pts',(6.91375968328197,0.816623019912162,12.2391739793356));
#19839=CARTESIAN_POINT('Ctrl Pts',(6.88517841785667,0.880319454332546,12.2436232271972));
#19840=CARTESIAN_POINT('Ctrl Pts',(6.85322879026267,0.942559082802846,12.2480724750588));
#19841=CARTESIAN_POINT('Ctrl Pts',(6.81808935639918,1.002969304061,12.2525217229204));
#19842=CARTESIAN_POINT('Ctrl Pts',(6.78296049682802,1.0633613464452,12.2569696318973));
#19843=CARTESIAN_POINT('Ctrl Pts',(6.74464398165632,1.12192465379024,12.2614175408743));
#19844=CARTESIAN_POINT('Ctrl Pts',(6.70336394796837,1.17831187554046,12.2658654498513));
#19845=CARTESIAN_POINT('Ctrl Pts',(6.66208247919094,1.23470105757758,12.2703135134587));
#19846=CARTESIAN_POINT('Ctrl Pts',(6.61783757702986,1.28891361215761,12.274761577066));
#19847=CARTESIAN_POINT('Ctrl Pts',(6.57089523458937,1.34063322802947,12.2792096406734));
#19848=CARTESIAN_POINT('Ctrl Pts',(6.52390530755207,1.39240527113313,12.2836622132017));
#19849=CARTESIAN_POINT('Ctrl Pts',(6.47421281053821,1.44167897015133,12.2881147857301));
#19850=CARTESIAN_POINT('Ctrl Pts',(6.42212171514428,1.48817375504167,12.2925673582585));
#19851=CARTESIAN_POINT('Ctrl Pts',(6.370001166536,1.53469482889475,12.297022448349));
#19852=CARTESIAN_POINT('Ctrl Pts',(6.31547969951562,1.57843355534781,12.3014775384396));
#19853=CARTESIAN_POINT('Ctrl Pts',(6.25889346380344,1.61915041291627,12.3059326285302));
#19854=CARTESIAN_POINT('Ctrl Pts',(6.20221252669866,1.65993541325949,12.3103951745547));
#19855=CARTESIAN_POINT('Ctrl Pts',(6.14346033266793,1.69768818583729,12.3148577205792));
#19856=CARTESIAN_POINT('Ctrl Pts',(6.08300030721383,1.73221362375885,12.3193202666037));
#19857=CARTESIAN_POINT('Ctrl Pts',(6.05337263044726,1.74913238135581,12.3215070812829));
#19858=CARTESIAN_POINT('Ctrl Pts',(6.02333518917303,1.76527685320593,12.3236938959622));
#19859=CARTESIAN_POINT('Ctrl Pts',(5.99293249614417,1.78062830170724,12.3258807106414));
#19860=CARTESIAN_POINT('Ctrl Pts',(5.93089953607057,1.81195104640785,12.3303426373384));
#19861=CARTESIAN_POINT('Ctrl Pts',(5.86710968920218,1.84008796029356,12.3348045640354));
#19862=CARTESIAN_POINT('Ctrl Pts',(5.80192264234284,1.86484003173098,12.3392664907323));
#19863=CARTESIAN_POINT('Ctrl Pts',(5.7368312905586,1.88955576694135,12.3437218672874));
#19864=CARTESIAN_POINT('Ctrl Pts',(5.67034726249248,1.91089635161925,12.3481772438424));
#19865=CARTESIAN_POINT('Ctrl Pts',(5.60285331167373,1.92870939614636,12.3526326203974));
#19866=CARTESIAN_POINT('Ctrl Pts',(5.53543625303222,1.94650214724332,12.3570829211849));
#19867=CARTESIAN_POINT('Ctrl Pts',(5.46701202615253,1.96077521685046,12.3615332219724));
#19868=CARTESIAN_POINT('Ctrl Pts',(5.39798009560142,1.9714255125414,12.3659835227599));
#19869=CARTESIAN_POINT('Ctrl Pts',(5.32899007130282,1.98206934290569,12.3704311219653));
#19870=CARTESIAN_POINT('Ctrl Pts',(5.25939355597442,1.98909468865264,12.3748787211707));
#19871=CARTESIAN_POINT('Ctrl Pts',(5.18960031806416,1.99244951349425,12.3793263203761));
#19872=CARTESIAN_POINT('Ctrl Pts',(5.11982598868202,1.99580342943979,12.3837727146288));
#19873=CARTESIAN_POINT('Ctrl Pts',(5.04985552917746,1.9954887755675,12.3882191088814));
#19874=CARTESIAN_POINT('Ctrl Pts',(4.98010218929287,1.99150550955097,12.392665503134));
#19875=CARTESIAN_POINT('Ctrl Pts',(4.91034430162017,1.98752198383289,12.3971121872833));
#19876=CARTESIAN_POINT('Ctrl Pts',(4.84080404815237,1.97986940126113,12.4015588714326));
#19877=CARTESIAN_POINT('Ctrl Pts',(4.77189127271463,1.96859971804971,12.4060055555819));
#19878=CARTESIAN_POINT('Ctrl Pts',(4.70290534783468,1.95731807230978,12.4104569597916));
#19879=CARTESIAN_POINT('Ctrl Pts',(4.63454871228637,1.94241174169231,12.4149083640013));
#19880=CARTESIAN_POINT('Ctrl Pts',(4.56722176774901,1.92398397294287,12.419359768211));
#19881=CARTESIAN_POINT('Ctrl Pts',(4.49985495273736,1.90554529141719,12.4238138085064));
#19882=CARTESIAN_POINT('Ctrl Pts',(4.43351950537399,1.88358117388198,12.4282678488019));
#19883=CARTESIAN_POINT('Ctrl Pts',(4.36859875255737,1.85824415137874,12.4327218890973));
#19884=CARTESIAN_POINT('Ctrl Pts',(4.30356652679628,1.83286362364212,12.4371835772552));
#19885=CARTESIAN_POINT('Ctrl Pts',(4.23995428840741,1.80409883119403,12.4416452654131));
#19886=CARTESIAN_POINT('Ctrl Pts',(4.17812281934862,1.77214929713595,12.4461069535709));
#19887=CARTESIAN_POINT('Ctrl Pts',(4.14762977101178,1.7563929403616,12.4483072970972));
#19888=CARTESIAN_POINT('Ctrl Pts',(4.1175694080126,1.73986270713659,12.4505076406234));
#19889=CARTESIAN_POINT('Ctrl Pts',(4.08798234152434,1.72258636149036,12.4527079841497));
#19890=CARTESIAN_POINT('Ctrl Pts',(4.02872379827553,1.68798438173463,12.4571149486611));
#19891=CARTESIAN_POINT('Ctrl Pts',(3.97112187864988,1.65024433874099,12.4615219131726));
#19892=CARTESIAN_POINT('Ctrl Pts',(3.91553427760012,1.60955070019584,12.4659288776841));
#19893=CARTESIAN_POINT('Ctrl Pts',(3.86003112086898,1.56891888023099,12.4703291474811));
#19894=CARTESIAN_POINT('Ctrl Pts',(3.80653661376772,1.52534265688757,12.4747294172781));
#19895=CARTESIAN_POINT('Ctrl Pts',(3.75538257227053,1.47905160837924,12.4791296870752));
#19896=CARTESIAN_POINT('Ctrl Pts',(3.70428711683655,1.43281357641103,12.4835249173));
#19897=CARTESIAN_POINT('Ctrl Pts',(3.65552717687369,1.38386722368545,12.4879201475249));
#19898=CARTESIAN_POINT('Ctrl Pts',(3.60940280615803,1.33248336339328,12.4923153777497));
#19899=CARTESIAN_POINT('Ctrl Pts',(3.56330634682053,1.2811305971699,12.4967079482758));
#19900=CARTESIAN_POINT('Ctrl Pts',(3.51984262916518,1.22734361880134,12.5011005188019));
#19901=CARTESIAN_POINT('Ctrl Pts',(3.47927478295544,1.1714299803924,12.5054930893279));
#19902=CARTESIAN_POINT('Ctrl Pts',(3.43871700971986,1.11553022530949,12.5098845691811));
#19903=CARTESIAN_POINT('Ctrl Pts',(3.40105397551522,1.05750526279527,12.5142760490343));
#19904=CARTESIAN_POINT('Ctrl Pts',(3.36650723192758,0.997694063474245,12.5186675288875));
#19905=CARTESIAN_POINT('Ctrl Pts',(3.33195673872641,0.937876372401497,12.5230594853805));
#19906=CARTESIAN_POINT('Ctrl Pts',(3.30052345541993,0.876272494759972,12.5274514418734));
#19907=CARTESIAN_POINT('Ctrl Pts',(3.27238348676533,0.813246902420903,12.5318433983664));
#19908=CARTESIAN_POINT('Ctrl Pts',(3.24420912633263,0.750144282199782,12.5362407225694));
#19909=CARTESIAN_POINT('Ctrl Pts',(3.2193363165379,0.68561693831397,12.5406380467725));
#19910=CARTESIAN_POINT('Ctrl Pts',(3.19789297972795,0.620049323697209,12.5450353709755));
#19911=CARTESIAN_POINT('Ctrl Pts',(3.17643544802973,0.554438305156324,12.549435606084));
#19912=CARTESIAN_POINT('Ctrl Pts',(3.15841203243788,0.48778613016387,12.5538358411925));
#19913=CARTESIAN_POINT('Ctrl Pts',(3.14389992929858,0.420489447193765,12.558236076301));
#19914=CARTESIAN_POINT('Ctrl Pts',(3.12935926600675,0.353060322804765,12.5626449711733));
#19915=CARTESIAN_POINT('Ctrl Pts',(3.11834378409934,0.284984653093198,12.5670538660456));
#19916=CARTESIAN_POINT('Ctrl Pts',(3.11087893255167,0.216665428234485,12.5714627609179));
#19917=CARTESIAN_POINT('Ctrl Pts',(3.10632299192651,0.17496890821315,12.5741535931646));
#19918=CARTESIAN_POINT('Ctrl Pts',(3.10308859917712,0.133181711858857,12.5768444254112));
#19919=CARTESIAN_POINT('Ctrl Pts',(3.10117201157415,0.0913949674364949,
12.5795352576578));
#19920=CARTESIAN_POINT('Ctrl Pts',(3.09790982357712,0.0202705294624338,
12.5841152730161));
#19921=CARTESIAN_POINT('Ctrl Pts',(3.09845473118738,-0.0511425087401567,
12.5886952883743));
#19922=CARTESIAN_POINT('Ctrl Pts',(3.10283697426873,-0.122415934123722,
12.5932753037325));
#19923=CARTESIAN_POINT('Ctrl Pts',(3.10734547188689,-0.195742781269199,
12.5979872715423));
#19924=CARTESIAN_POINT('Ctrl Pts',(3.11591592914825,-0.26892136795584,12.602699239352));
#19925=CARTESIAN_POINT('Ctrl Pts',(3.12852366695523,-0.341481713416793,
12.6074112071617));
#19926=CARTESIAN_POINT('Ctrl Pts',(3.14073779752797,-0.411776761381121,
12.611976069706));
#19927=CARTESIAN_POINT('Ctrl Pts',(3.15674076481258,-0.481491110343606,
12.6165409322502));
#19928=CARTESIAN_POINT('Ctrl Pts',(3.17645751882798,-0.550201089646342,
12.6211057947944));
#19929=CARTESIAN_POINT('Ctrl Pts',(3.19615568536413,-0.618846294325737,
12.6256663539281));
#19930=CARTESIAN_POINT('Ctrl Pts',(3.21956055507191,-0.686488574425669,
12.6302269130617));
#19931=CARTESIAN_POINT('Ctrl Pts',(3.24654635307994,-0.752715882444068,
12.6347874721954));
#19932=CARTESIAN_POINT('Ctrl Pts',(3.27351392811627,-0.818898468480926,
12.6393449516743));
#19933=CARTESIAN_POINT('Ctrl Pts',(3.30405745206538,-0.883667560659087,
12.6439024311533));
#19934=CARTESIAN_POINT('Ctrl Pts',(3.33800223095384,-0.946628964804647,
12.6484599106322));
#19935=CARTESIAN_POINT('Ctrl Pts',(3.37193315718283,-1.00956467478106,12.6530155302313));
#19936=CARTESIAN_POINT('Ctrl Pts',(3.40926236073151,-1.0706937633267,12.6575711498303));
#19937=CARTESIAN_POINT('Ctrl Pts',(3.44976881160282,-1.12964584030406,12.6621267694294));
#19938=CARTESIAN_POINT('Ctrl Pts',(3.49028059898438,-1.18860568390513,12.6666829892072));
#19939=CARTESIAN_POINT('Ctrl Pts',(3.53397021691296,-1.24538756331038,12.671239208985));
#19940=CARTESIAN_POINT('Ctrl Pts',(3.58057339540124,-1.29965019147034,12.6757954287628));
#19941=CARTESIAN_POINT('Ctrl Pts',(3.62717973921168,-1.3539165051879,12.6803519580024));
#19942=CARTESIAN_POINT('Ctrl Pts',(3.67669973409684,-1.40566288633933,12.684908487242));
#19943=CARTESIAN_POINT('Ctrl Pts',(3.72883010209269,-1.45458262289131,12.6894650164816));
#19944=CARTESIAN_POINT('Ctrl Pts',(3.78099529562535,-1.50353504012734,12.694024589697));
#19945=CARTESIAN_POINT('Ctrl Pts',(3.83577400428353,-1.54965673795645,12.6985841629123));
#19946=CARTESIAN_POINT('Ctrl Pts',(3.89282823149158,-1.59267986335712,12.7031437361277));
#19947=CARTESIAN_POINT('Ctrl Pts',(3.90625389326459,-1.60280380961513,12.7042166678072));
#19948=CARTESIAN_POINT('Ctrl Pts',(3.91980542131159,-1.61275636221494,12.7052895994866));
#19949=CARTESIAN_POINT('Ctrl Pts',(3.93347817078409,-1.62253437445176,12.7063625311661));
#19950=CARTESIAN_POINT('Ctrl Pts',(5.96741924226898,-1.78935549366613,-5.55880302681794));
#19951=CARTESIAN_POINT('Ctrl Pts',(6.5615443607172,-1.49929406993443,-5.51652726898187));
#19952=CARTESIAN_POINT('Ctrl Pts',(7.42803687527648,-0.286026890556653,
-5.43197575330973));
#19953=CARTESIAN_POINT('Ctrl Pts',(6.60117793883817,1.80796350105253,-5.30514847980151));
#19954=CARTESIAN_POINT('Ctrl Pts',(4.3963971709158,2.24586678413418,-5.17832120629329));
#19955=CARTESIAN_POINT('Ctrl Pts',(2.82926100857112,0.636515102147664,-5.05149393278508));
#19956=CARTESIAN_POINT('Ctrl Pts',(3.32878390476465,-1.5553570121133,-4.92466665927686));
#19957=CARTESIAN_POINT('Ctrl Pts',(5.43978137117777,-2.32666155138565,-4.79783938576864));
#19958=CARTESIAN_POINT('Ctrl Pts',(7.2348341668827,-0.974507642748168,-4.67101211226043));
#19959=CARTESIAN_POINT('Ctrl Pts',(7.07556887268865,1.26742862746759,-4.54418483875221));
#19960=CARTESIAN_POINT('Ctrl Pts',(5.10725347901043,2.35229469782244,-4.417357565244));
#19961=CARTESIAN_POINT('Ctrl Pts',(3.12670289415786,1.2899543892979,-4.29053029173577));
#19962=CARTESIAN_POINT('Ctrl Pts',(2.94180830639893,-0.949937059360794,
-4.16370301822756));
#19963=CARTESIAN_POINT('Ctrl Pts',(4.72136534354493,-2.3226730290144,-4.03687574471934));
#19964=CARTESIAN_POINT('Ctrl Pts',(6.84091687949711,-1.57519194182562,-3.91004847121113));
#19965=CARTESIAN_POINT('Ctrl Pts',(7.36565906395742,0.610189633448571,-3.78322119770291));
#19966=CARTESIAN_POINT('Ctrl Pts',(5.81658455864063,2.23856420545701,-3.65639392419469));
#19967=CARTESIAN_POINT('Ctrl Pts',(3.60774963453304,1.82349219851761,-3.52956665068648));
#19968=CARTESIAN_POINT('Ctrl Pts',(2.75546340395978,-0.256134521428759,
-3.40273937717826));
#19969=CARTESIAN_POINT('Ctrl Pts',(4.03772598570737,-2.10195142318311,-3.27591210367005));
#19970=CARTESIAN_POINT('Ctrl Pts',(6.28403841692564,-2.02902611036282,-3.14908483016182));
#19971=CARTESIAN_POINT('Ctrl Pts',(7.44388010034515,-0.103927350902949,
-3.02225755665361));
#19972=CARTESIAN_POINT('Ctrl Pts',(6.45850272749029,1.91604025675891,-2.89543028314539));
#19973=CARTESIAN_POINT('Ctrl Pts',(4.22739682589132,2.18697238579333,-2.76860300963718));
#19974=CARTESIAN_POINT('Ctrl Pts',(2.78720196805409,0.461551691566315,-2.64177573612896));
#19975=CARTESIAN_POINT('Ctrl Pts',(3.45258361826661,-1.6851911952421,-2.51494846262075));
#19976=CARTESIAN_POINT('Ctrl Pts',(5.61615571900432,-2.2936265153134,-2.38812118911253));
#19977=CARTESIAN_POINT('Ctrl Pts',(7.30292614602958,-0.808351017512908,
-2.26129391560431));
#19978=CARTESIAN_POINT('Ctrl Pts',(6.97314574407777,1.41481848995056,-2.13446664209609));
#19979=CARTESIAN_POINT('Ctrl Pts',(4.92785079394974,2.34648706910725,-2.00763936858788));
#19980=CARTESIAN_POINT('Ctrl Pts',(3.03406547309841,1.13619167817969,-1.88081209507966));
#19981=CARTESIAN_POINT('Ctrl Pts',(3.02051012162903,-1.11126333281937,-1.75398482157145));
#19982=CARTESIAN_POINT('Ctrl Pts',(4.89955858751159,-2.34431427954153,-1.62715754806323));
#19983=CARTESIAN_POINT('Ctrl Pts',(6.95594290088628,-1.43738466260644,-1.50033027455501));
#19984=CARTESIAN_POINT('Ctrl Pts',(7.31251608517135,0.781645156597075,-1.3735030010468));
#19985=CARTESIAN_POINT('Ctrl Pts',(5.6437843742328,2.28715910579401,-1.24667572753858));
#19986=CARTESIAN_POINT('Ctrl Pts',(3.47303048594182,1.70486594012406,-1.11984845403036));
#19987=CARTESIAN_POINT('Ctrl Pts',(2.78180235944796,-0.433694662582063,
-0.993021180522151));
#19988=CARTESIAN_POINT('Ctrl Pts',(4.20107970964125,-2.17636203690783,-0.866193907013934));
#19989=CARTESIAN_POINT('Ctrl Pts',(6.43529138793569,-1.93236213755744,-0.739366633505718));
#19990=CARTESIAN_POINT('Ctrl Pts',(7.44496273503322,0.0755725090779332,
-0.612539359997501));
#19991=CARTESIAN_POINT('Ctrl Pts',(6.308426772541,2.01452165236963,-0.485712086489285));
#19992=CARTESIAN_POINT('Ctrl Pts',(4.06315739668914,2.11453767194281,-0.358884812981069));
#19993=CARTESIAN_POINT('Ctrl Pts',(2.75872315992675,0.284322084567546,-0.232057539472851));
#19994=CARTESIAN_POINT('Ctrl Pts',(3.58586198401954,-1.80543367627818,-0.105230265964635));
#19995=CARTESIAN_POINT('Ctrl Pts',(5.78952962322882,-2.24711988866344,0.0215970075435808));
#19996=CARTESIAN_POINT('Ctrl Pts',(7.35813319611717,-0.637548329076448,
0.148424281051797));
#19997=CARTESIAN_POINT('Ctrl Pts',(6.85979081411103,1.55400195430878,0.275251554560013));
#19998=CARTESIAN_POINT('Ctrl Pts',(4.74940863924933,2.32699927017435,0.402078828068231));
#19999=CARTESIAN_POINT('Ctrl Pts',(2.95342498034503,0.975821831324032,0.528906101576446));
#20000=CARTESIAN_POINT('Ctrl Pts',(3.11128304523419,-1.26612344134854,0.655733375084663));
#20001=CARTESIAN_POINT('Ctrl Pts',(5.07888389905091,-2.35230236508492,0.782560648592879));
#20002=CARTESIAN_POINT('Ctrl Pts',(7.06012553411309,-1.29120889238538,0.909387922101095));
#20003=CARTESIAN_POINT('Ctrl Pts',(7.24645411109106,0.948549897241488,1.03621519560932));
#20004=CARTESIAN_POINT('Ctrl Pts',(5.46778171273805,2.32243572715841,1.16304246911752));
#20005=CARTESIAN_POINT('Ctrl Pts',(3.34774916005368,1.57631258057466,1.28986974262575));
#20006=CARTESIAN_POINT('Ctrl Pts',(2.82160399922678,-0.608729534362231,
1.41669701613396));
#20007=CARTESIAN_POINT('Ctrl Pts',(4.36963184197595,-2.23809983370575,1.54352428964218));
#20008=CARTESIAN_POINT('Ctrl Pts',(6.57873312041059,-1.82444621541158,1.6703515631504));
#20009=CARTESIAN_POINT('Ctrl Pts',(7.43235491747289,0.254632330937633,1.7971788366586));
#20010=CARTESIAN_POINT('Ctrl Pts',(6.15127830746928,2.10127265693809,1.92400611016684));
#20011=CARTESIAN_POINT('Ctrl Pts',(3.90491946886846,2.02979019370868,2.05083338367504));
#20012=CARTESIAN_POINT('Ctrl Pts',(2.74384145776938,0.105436892869242,2.17766065718327));
#20013=CARTESIAN_POINT('Ctrl Pts',(3.72792109968031,-1.91516327358771,2.30448793069147));
#20014=CARTESIAN_POINT('Ctrl Pts',(5.95885251252833,-2.18752847965755,2.4313152041997));
#20015=CARTESIAN_POINT('Ctrl Pts',(7.40015538993177,-0.463033252091554,
2.55814247770792));
#20016=CARTESIAN_POINT('Ctrl Pts',(6.73615283189305,1.68413660081422,2.68496975121613));
#20017=CARTESIAN_POINT('Ctrl Pts',(4.57297200352591,2.29396155774392,2.81179702472434));
#20018=CARTESIAN_POINT('Ctrl Pts',(2.88524786256229,0.80976985910186,2.93862429823255));
#20019=CARTESIAN_POINT('Ctrl Pts',(3.21360015010372,-1.41361102360262,3.06545157174077));
#20020=CARTESIAN_POINT('Ctrl Pts',(5.25829622386344,-2.34659319934927,3.19227884524899));
#20021=CARTESIAN_POINT('Ctrl Pts',(7.15285858356203,-1.13751452551417,3.31910611875722));
#20022=CARTESIAN_POINT('Ctrl Pts',(7.16785757819435,1.10993131464959,3.44593339226543));
#20023=CARTESIAN_POINT('Ctrl Pts',(5.28960154650705,2.34418900805874,3.57276066577364));
#20024=CARTESIAN_POINT('Ctrl Pts',(3.23263509388115,1.43858049049663,3.69958793928185));
#20025=CARTESIAN_POINT('Ctrl Pts',(2.87463659605508,-0.780219827211948,
3.82641521279009));
#20026=CARTESIAN_POINT('Ctrl Pts',(4.54240090039093,-2.28680537058231,3.95324248629829));
#20027=CARTESIAN_POINT('Ctrl Pts',(6.71352837509979,-1.70590670224695,4.08006975980651));
#20028=CARTESIAN_POINT('Ctrl Pts',(7.40613005693279,0.432209450966328,4.20689703331472));
#20029=CARTESIAN_POINT('Ctrl Pts',(5.98797239666618,2.17578813428881,4.33372430682294));
#20030=CARTESIAN_POINT('Ctrl Pts',(3.7536044467024,1.93322342439896,4.46055158033115));
#20031=CARTESIAN_POINT('Ctrl Pts',(2.74264351715072,-0.07406224865045,4.58737885383938));
#20032=CARTESIAN_POINT('Ctrl Pts',(3.87793376704564,-2.0137410423694,4.71420612734759));
#20033=CARTESIAN_POINT('Ctrl Pts',(6.12313843469951,-2.11519928330928,4.8410334008558));
#20034=CARTESIAN_POINT('Ctrl Pts',(7.42874803580416,-0.285821972907499,
4.96786067436402));
#20035=CARTESIAN_POINT('Ctrl Pts',(6.60295173065374,1.80446466693628,5.09468794787225));
#20036=CARTESIAN_POINT('Ctrl Pts',(4.39956826187594,2.24756630745012,5.22151522138046));
#20037=CARTESIAN_POINT('Ctrl Pts',(2.82993110916943,0.639002667691711,5.34834249488867));
#20038=CARTESIAN_POINT('Ctrl Pts',(3.32686565266144,-1.55286727228962,5.47516976839688));
#20039=CARTESIAN_POINT('Ctrl Pts',(5.43675085965053,-2.3272200262965,5.6019970419051));
#20040=CARTESIAN_POINT('Ctrl Pts',(7.23360207278054,-0.977196510878107,
5.72882431541332));
#20041=CARTESIAN_POINT('Ctrl Pts',(7.07718414723108,1.26484969892137,5.85565158892153));
#20042=CARTESIAN_POINT('Ctrl Pts',(5.11028140309013,2.35229228103794,5.98247886242977));
#20043=CARTESIAN_POINT('Ctrl Pts',(3.12835858658117,1.29247167182591,6.10930613593796));
#20044=CARTESIAN_POINT('Ctrl Pts',(2.94059134575166,-0.947166968129349,
6.23613340944619));
#20045=CARTESIAN_POINT('Ctrl Pts',(4.71838086574373,-2.32219503944855,6.36296068295439));
#20046=CARTESIAN_POINT('Ctrl Pts',(6.83889225100422,-1.57743384329904,6.48978795646262));
#20047=CARTESIAN_POINT('Ctrl Pts',(7.36644085848617,0.60726985309855,6.61661522997083));
#20048=CARTESIAN_POINT('Ctrl Pts',(5.81945995619197,2.23763418730316,6.74344250347906));
#20049=CARTESIAN_POINT('Ctrl Pts',(3.61009342435358,1.82539966388007,6.87026977698727));
#20050=CARTESIAN_POINT('Ctrl Pts',(2.75513631357441,-0.253130132162693,
6.99709705049549));
#20051=CARTESIAN_POINT('Ctrl Pts',(4.03502647545116,-2.1005929728825,7.1239243240037));
#20052=CARTESIAN_POINT('Ctrl Pts',(6.28143076716157,-2.03055346621384,7.25075159751192));
#20053=CARTESIAN_POINT('Ctrl Pts',(7.44374464125381,-0.106946377330505,
7.37757887102014));
#20054=CARTESIAN_POINT('Ctrl Pts',(6.46096312877579,1.91428549285182,7.50440614452834));
#20055=CARTESIAN_POINT('Ctrl Pts',(4.23020712914702,2.18808367478468,7.63123341803657));
#20056=CARTESIAN_POINT('Ctrl Pts',(2.78779682479175,0.464514619539295,7.75806069154478));
#20057=CARTESIAN_POINT('Ctrl Pts',(3.45042001777526,-1.6830813104319,7.88488796505301));
#20058=CARTESIAN_POINT('Ctrl Pts',(5.61320868064904,-2.29429565422208,8.0117152385612));
#20059=CARTESIAN_POINT('Ctrl Pts',(7.30188583948063,-0.811188366278425,
8.13854251206945));
#20060=CARTESIAN_POINT('Ctrl Pts',(6.97496180167311,1.41240297383033,8.26536978557763));
#20061=CARTESIAN_POINT('Ctrl Pts',(4.93086544802557,2.34669836144671,8.39219705908588));
#20062=CARTESIAN_POINT('Ctrl Pts',(3.03552683115188,1.13883690345341,8.51902433259408));
#20063=CARTESIAN_POINT('Ctrl Pts',(3.01908419956648,-1.10859883848275,8.64585160610229));
#20064=CARTESIAN_POINT('Ctrl Pts',(4.89654702206317,-2.34406276936477,8.77267887961052));
#20065=CARTESIAN_POINT('Ctrl Pts',(6.95409476521605,-1.4397757247852,8.89950615311873));
#20066=CARTESIAN_POINT('Ctrl Pts',(7.31351842887804,0.778794175853053,9.02633342662694));
#20067=CARTESIAN_POINT('Ctrl Pts',(5.64672221925978,2.28645069189862,9.15316070013516));
#20068=CARTESIAN_POINT('Ctrl Pts',(3.47522205400328,1.70694676033461,9.27998797364338));
#20069=CARTESIAN_POINT('Ctrl Pts',(2.78124710252401,-0.430724060710163,
9.4068152471516));
#20070=CARTESIAN_POINT('Ctrl Pts',(4.1982844878738,-2.17521333450196,9.53364252065981));
#20071=CARTESIAN_POINT('Ctrl Pts',(6.43280778728865,-1.93408391246274,9.66046979416803));
#20072=CARTESIAN_POINT('Ctrl Pts',(7.44505788272711,0.0725519555479146,
9.78729706767624));
#20073=CARTESIAN_POINT('Ctrl Pts',(6.31101381278495,2.01295960551136,9.91412434118447));
#20074=CARTESIAN_POINT('Ctrl Pts',(4.06587478177254,2.11586001424485,10.0409516146927));
#20075=CARTESIAN_POINT('Ctrl Pts',(2.75909035112716,0.287321757942756,10.1677788882009));
#20076=CARTESIAN_POINT('Ctrl Pts',(3.5835438040437,-1.80349494092047,10.2946061617091));
#20077=CARTESIAN_POINT('Ctrl Pts',(5.78664217907986,-2.24801174578714,10.4214334352174));
#20078=CARTESIAN_POINT('Ctrl Pts',(7.35731229095528,-0.640456843765642,
10.5482607087256));
#20079=CARTESIAN_POINT('Ctrl Pts',(6.86178573958764,1.55173214216356,10.6750879822338));
#20080=CARTESIAN_POINT('Ctrl Pts',(4.75239846900008,2.32743945525609,10.801915255742));
#20081=CARTESIAN_POINT('Ctrl Pts',(2.95468025641726,0.978571486204148,10.9287425292502));
#20082=CARTESIAN_POINT('Ctrl Pts',(3.10965833359497,-1.26357676609641,11.0555698027584));
#20083=CARTESIAN_POINT('Ctrl Pts',(5.07586147928159,-2.35227869001964,11.1823970762667));
#20084=CARTESIAN_POINT('Ctrl Pts',(7.05846594952206,-1.29373874962098,11.3092243497749));
#20085=CARTESIAN_POINT('Ctrl Pts',(7.24766931928765,0.945792852126664,11.4360516232831));
#20086=CARTESIAN_POINT('Ctrl Pts',(5.47076809243279,2.32193586078442,11.5628788967913));
#20087=CARTESIAN_POINT('Ctrl Pts',(3.34976983211822,1.57858785389917,11.6897061702995));
#20088=CARTESIAN_POINT('Ctrl Pts',(2.82083498267555,-0.605873543948998,
11.8165334438077));
#20089=CARTESIAN_POINT('Ctrl Pts',(4.36673594724824,-2.23704641637698,11.943360717316));
#20090=CARTESIAN_POINT('Ctrl Pts',(6.57642846184293,-1.82658327984848,12.0701879908242));
#20091=CARTESIAN_POINT('Ctrl Pts',(7.43260311629662,0.252068073834375,12.1970152643324));
#20092=CARTESIAN_POINT('Ctrl Pts',(6.15412356552886,2.09907067965551,12.3238425378406));
#20093=CARTESIAN_POINT('Ctrl Pts',(3.90724904943681,2.03294633564993,12.4506698113488));
#20094=CARTESIAN_POINT('Ctrl Pts',(2.74435016673355,0.104853876027658,12.5775143854051));
#20095=CARTESIAN_POINT('Ctrl Pts',(3.39801752208532,-1.23561899131413,12.6620832016253));
#20096=CARTESIAN_POINT('Ctrl Pts',(3.93619204088349,-1.62013490387918,12.7043762600095));
#20097=CARTESIAN_POINT('Ctrl Pts',(6.03504684936144,-1.92787532700788,-5.46980632749697));
#20098=CARTESIAN_POINT('Ctrl Pts',(6.67516512718069,-1.61535930427873,-5.4275305696609));
#20099=CARTESIAN_POINT('Ctrl Pts',(7.60873564783407,-0.308169163208136,
-5.34297905398876));
#20100=CARTESIAN_POINT('Ctrl Pts',(6.7178668695963,1.94792384081748,-5.21615178048054));
#20101=CARTESIAN_POINT('Ctrl Pts',(4.3424068455905,2.4197266424727,-5.08932450697231));
#20102=CARTESIAN_POINT('Ctrl Pts',(2.65395357169351,0.685789808141594,-4.96249723346412));
#20103=CARTESIAN_POINT('Ctrl Pts',(3.19214616129121,-1.67576226130358,-4.83566995995589));
#20104=CARTESIAN_POINT('Ctrl Pts',(5.46656281314146,-2.50677599565422,-4.70884268644769));
#20105=CARTESIAN_POINT('Ctrl Pts',(7.40057648888444,-1.04994745151819,-4.58201541293946));
#20106=CARTESIAN_POINT('Ctrl Pts',(7.22898194983825,1.36554440315936,-4.45518813943125));
#20107=CARTESIAN_POINT('Ctrl Pts',(5.10829285442139,2.53439348739581,-4.32836086592303));
#20108=CARTESIAN_POINT('Ctrl Pts',(2.97442140185426,1.38981395753714,-4.20153359241481));
#20109=CARTESIAN_POINT('Ctrl Pts',(2.77521352220177,-1.02347477929045,-4.0747063189066));
#20110=CARTESIAN_POINT('Ctrl Pts',(4.69253186227509,-2.50247870878307,-3.94787904539838));
#20111=CARTESIAN_POINT('Ctrl Pts',(6.97616478203201,-1.69713267749013,-3.82105177189016));
#20112=CARTESIAN_POINT('Ctrl Pts',(7.54152896709318,0.657426399217776,-3.69422449838195));
#20113=CARTESIAN_POINT('Ctrl Pts',(5.87253556188757,2.41185874740932,-3.56739722487373));
#20114=CARTESIAN_POINT('Ctrl Pts',(3.49270753626949,1.96465466530119,-3.44056995136552));
#20115=CARTESIAN_POINT('Ctrl Pts',(2.57444305428872,-0.275962728482613,
-3.3137426778573));
#20116=CARTESIAN_POINT('Ctrl Pts',(3.95596975641528,-2.26467032496782,-3.18691540434908));
#20117=CARTESIAN_POINT('Ctrl Pts',(6.3761765449635,-2.18609962630105,-3.06008813084087));
#20118=CARTESIAN_POINT('Ctrl Pts',(7.62580534852698,-0.111972705432947,
-2.93326085733265));
#20119=CARTESIAN_POINT('Ctrl Pts',(6.56414670571223,2.0643671699865,-2.80643358382443));
#20120=CARTESIAN_POINT('Ctrl Pts',(4.1603236337403,2.35627303704761,-2.67960631031622));
#20121=CARTESIAN_POINT('Ctrl Pts',(2.60863860394261,0.497281910419246,-2.552779036808));
#20122=CARTESIAN_POINT('Ctrl Pts',(3.32552961359897,-1.81564733117496,-2.42595176329978));
#20123=CARTESIAN_POINT('Ctrl Pts',(5.65659087335395,-2.47118360990644,-2.29912448979157));
#20124=CARTESIAN_POINT('Ctrl Pts',(7.47393968978501,-0.870928101062764,
-2.17229721628335));
#20125=CARTESIAN_POINT('Ctrl Pts',(7.11862991344148,1.52434419466967,-2.04546994277514));
#20126=CARTESIAN_POINT('Ctrl Pts',(4.91500202353184,2.52813627123722,-1.91864266926692));
#20127=CARTESIAN_POINT('Ctrl Pts',(2.87461261648416,1.22414797443433,-1.7918153957587));
#20128=CARTESIAN_POINT('Ctrl Pts',(2.86000790113313,-1.19728984471475,-1.66498812225048));
#20129=CARTESIAN_POINT('Ctrl Pts',(4.88451962529862,-2.52579527895851,-1.53816084874227));
#20130=CARTESIAN_POINT('Ctrl Pts',(7.10009534216109,-1.54865728820657,-1.41133357523405));
#20131=CARTESIAN_POINT('Ctrl Pts',(7.48427201733219,0.842154852522489,-1.28450630172584));
#20132=CARTESIAN_POINT('Ctrl Pts',(5.68635835271843,2.46421553716391,-1.15767902821762));
#20133=CARTESIAN_POINT('Ctrl Pts',(3.34755933985805,1.83684516210202,-1.0308517547094));
#20134=CARTESIAN_POINT('Ctrl Pts',(2.60282099405786,-0.467268378143176,
-0.904024481201181));
#20135=CARTESIAN_POINT('Ctrl Pts',(4.1319692238558,-2.34484130651688,-0.777197207692966));
#20136=CARTESIAN_POINT('Ctrl Pts',(6.53913850080685,-2.08195258070742,-0.650369934184749));
#20137=CARTESIAN_POINT('Ctrl Pts',(7.62697179349039,0.0814228230036674,
-0.523542660676532));
#20138=CARTESIAN_POINT('Ctrl Pts',(6.40245288257421,2.17047233100077,-0.396715387168316));
#20139=CARTESIAN_POINT('Ctrl Pts',(3.98336989570362,2.27823091621384,-0.2698881136601));
#20140=CARTESIAN_POINT('Ctrl Pts',(2.57795515857602,0.306332382638052,-0.143060840151882));
#20141=CARTESIAN_POINT('Ctrl Pts',(3.46912549148267,-1.94519817407244,-0.0162335666436664));
#20142=CARTESIAN_POINT('Ctrl Pts',(5.84338621585831,-2.42107675390258,0.11059370686455));
#20143=CARTESIAN_POINT('Ctrl Pts',(7.53342049732578,-0.686903020530217,
0.237420980372767));
#20144=CARTESIAN_POINT('Ctrl Pts',(6.99649980936145,1.67430230406352,0.364248253880983));
#20145=CARTESIAN_POINT('Ctrl Pts',(4.72274608078444,2.50713985835369,0.491075527389199));
#20146=CARTESIAN_POINT('Ctrl Pts',(2.78772948069178,1.05136337570955,0.617902800897417));
#20147=CARTESIAN_POINT('Ctrl Pts',(2.95780785223184,-1.36413817833427,0.744730074405631));
#20148=CARTESIAN_POINT('Ctrl Pts',(5.07772709293065,-2.53440174820603,0.87155734791385));
#20149=CARTESIAN_POINT('Ctrl Pts',(7.21234309215354,-1.39116557579219,0.998384621422065));
#20150=CARTESIAN_POINT('Ctrl Pts',(7.41309597079834,1.0219802324361,1.12521189493028));
#20151=CARTESIAN_POINT('Ctrl Pts',(5.49673075228657,2.50222303661797,1.2520391684385));
#20152=CARTESIAN_POINT('Ctrl Pts',(3.21257957872646,1.69834006853254,1.37886644194671));
#20153=CARTESIAN_POINT('Ctrl Pts',(2.6457038083313,-0.655853269108355,1.50569371545493));
#20154=CARTESIAN_POINT('Ctrl Pts',(4.3135695254129,-2.41135842712921,1.63252098896314));
#20155=CARTESIAN_POINT('Ctrl Pts',(6.69368452471353,-1.96568253574837,1.75934826247136));
#20156=CARTESIAN_POINT('Ctrl Pts',(7.61338796373266,0.274344248535754,1.88617553597958));
#20157=CARTESIAN_POINT('Ctrl Pts',(6.23313904328329,2.2639390132183,2.01300280948779));
#20158=CARTESIAN_POINT('Ctrl Pts',(3.81288225480597,2.1869228598259,2.13983008299601));
#20159=CARTESIAN_POINT('Ctrl Pts',(2.56192141541284,0.113599105956597,2.26665735650423));
#20160=CARTESIAN_POINT('Ctrl Pts',(3.62218186570703,-2.06342229669333,2.39348463001244));
#20161=CARTESIAN_POINT('Ctrl Pts',(6.02581694118578,-2.35687217994802,2.52031190352066));
#20162=CARTESIAN_POINT('Ctrl Pts',(7.57869576595109,-0.49887816336741,2.64713917702888));
#20163=CARTESIAN_POINT('Ctrl Pts',(6.86329060848278,1.81451109715958,2.77396645053709));
#20164=CARTESIAN_POINT('Ctrl Pts',(4.53265091076624,2.4715445890621,2.90079372404531));
#20165=CARTESIAN_POINT('Ctrl Pts',(2.71427455029638,0.872456779797623,3.02762099755352));
#20166=CARTESIAN_POINT('Ctrl Pts',(3.06804565724436,-1.52304325442127,3.15444827106175));
#20167=CARTESIAN_POINT('Ctrl Pts',(5.27102830981658,-2.52825061736673,3.28127554456996));
#20168=CARTESIAN_POINT('Ctrl Pts',(7.31225490881806,-1.22557322768701,3.40810281807818));
#20169=CARTESIAN_POINT('Ctrl Pts',(7.32841502444848,1.19585471068256,3.53493009158639));
#20170=CARTESIAN_POINT('Ctrl Pts',(5.30475707938881,2.52566030980246,3.66175736509461));
#20171=CARTESIAN_POINT('Ctrl Pts',(3.08855415798074,1.54994568902632,3.78858463860283));
#20172=CARTESIAN_POINT('Ctrl Pts',(2.70284183110785,-0.840619183750031,
3.91541191211104));
#20173=CARTESIAN_POINT('Ctrl Pts',(4.49971319902478,-2.46383441815802,4.04223918561925));
#20174=CARTESIAN_POINT('Ctrl Pts',(6.83891471884371,-1.83796649300864,4.16906645912748));
#20175=CARTESIAN_POINT('Ctrl Pts',(7.58513295137294,0.465668191461714,4.29589373263569));
#20176=CARTESIAN_POINT('Ctrl Pts',(6.05719109034367,2.34422297622799,4.42272100614391));
#20177=CARTESIAN_POINT('Ctrl Pts',(3.64985344422461,2.08288054256695,4.54954827965212));
#20178=CARTESIAN_POINT('Ctrl Pts',(2.56063073831145,-0.0797956484004017,
4.67637555316034));
#20179=CARTESIAN_POINT('Ctrl Pts',(3.78380750196318,-2.16963129143944,4.80320282666856));
#20180=CARTESIAN_POINT('Ctrl Pts',(6.20282077136359,-2.27894374506981,4.93003010017677));
#20181=CARTESIAN_POINT('Ctrl Pts',(7.60950186161309,-0.307948382216727,
5.056857373685));
#20182=CARTESIAN_POINT('Ctrl Pts',(6.71977797641024,1.94415415056313,5.18368464719321));
#20183=CARTESIAN_POINT('Ctrl Pts',(4.34582342102416,2.42155773142069,5.31051192070143));
#20184=CARTESIAN_POINT('Ctrl Pts',(2.65467554696042,0.688469944231741,5.43733919420963));
#20185=CARTESIAN_POINT('Ctrl Pts',(3.19007941104852,-1.67307978261573,5.56416646771786));
#20186=CARTESIAN_POINT('Ctrl Pts',(5.46329769985222,-2.50737770392584,5.69099374122607));
#20187=CARTESIAN_POINT('Ctrl Pts',(7.39924901436718,-1.05284447368267,5.81782101473429));
#20188=CARTESIAN_POINT('Ctrl Pts',(7.23072226804094,1.36276583135963,5.94464828824251));
#20189=CARTESIAN_POINT('Ctrl Pts',(5.11155517996038,2.53439088352015,6.07147556175072));
#20190=CARTESIAN_POINT('Ctrl Pts',(2.97620526681754,1.39252611109973,6.19830283525895));
#20191=CARTESIAN_POINT('Ctrl Pts',(2.77390235266945,-1.02049024627978,6.32513010876715));
#20192=CARTESIAN_POINT('Ctrl Pts',(4.68931634633245,-2.50196371648903,6.45195738227537));
#20193=CARTESIAN_POINT('Ctrl Pts',(6.97398342045709,-1.69954813185427,6.5787846557836));
#20194=CARTESIAN_POINT('Ctrl Pts',(7.54237128288121,0.654280589166612,6.7056119292918));
#20195=CARTESIAN_POINT('Ctrl Pts',(5.87563355332317,2.41085673352286,6.83243920280003));
#20196=CARTESIAN_POINT('Ctrl Pts',(3.49523276648935,1.96670979376639,6.95926647630824));
#20197=CARTESIAN_POINT('Ctrl Pts',(2.57409064277192,-0.272725759663801,
7.08609374981645));
#20198=CARTESIAN_POINT('Ctrl Pts',(3.95306126828289,-2.26320671260751,7.21292102332467));
#20199=CARTESIAN_POINT('Ctrl Pts',(6.37336702854295,-2.18774521974024,7.33974829683289));
#20200=CARTESIAN_POINT('Ctrl Pts',(7.62565940310645,-0.115225444523568,
7.46657557034111));
#20201=CARTESIAN_POINT('Ctrl Pts',(6.56679757467015,2.06247656409339,7.59340284384931));
#20202=CARTESIAN_POINT('Ctrl Pts',(4.16335149171894,2.35747035453718,7.72023011735755));
#20203=CARTESIAN_POINT('Ctrl Pts',(2.60927951047665,0.500474208291315,7.84705739086575));
#20204=CARTESIAN_POINT('Ctrl Pts',(3.3231985217508,-1.81337411331366,7.97388466437398));
#20205=CARTESIAN_POINT('Ctrl Pts',(5.6534156951666,-2.47190454903617,8.10071193788218));
#20206=CARTESIAN_POINT('Ctrl Pts',(7.47281884971977,-0.873985098232146,
8.2275392113904));
#20207=CARTESIAN_POINT('Ctrl Pts',(7.12058655796674,1.52174168558375,8.35436648489863));
#20208=CARTESIAN_POINT('Ctrl Pts',(4.91825005179277,2.52836392040445,8.48119375840682));
#20209=CARTESIAN_POINT('Ctrl Pts',(2.87618710302144,1.22699797520702,8.60802103191507));
#20210=CARTESIAN_POINT('Ctrl Pts',(2.85847159380217,-1.19441908319826,8.73484830542326));
#20211=CARTESIAN_POINT('Ctrl Pts',(4.88127492476582,-2.52552429856026,8.86167557893149));
#20212=CARTESIAN_POINT('Ctrl Pts',(7.09810413629271,-1.55123345029179,8.98850285243972));
#20213=CARTESIAN_POINT('Ctrl Pts',(7.48535195572798,0.839083168078771,9.11533012594791));
#20214=CARTESIAN_POINT('Ctrl Pts',(5.689523625892,2.46345228264291,9.24215739945616));
#20215=CARTESIAN_POINT('Ctrl Pts',(3.34992056433698,1.8390870653784,9.36898467296433));
#20216=CARTESIAN_POINT('Ctrl Pts',(2.60222275288801,-0.464067812310691,
9.4958119464726));
#20217=CARTESIAN_POINT('Ctrl Pts',(4.12895761487251,-2.34360367931858,9.62263921998077));
#20218=CARTESIAN_POINT('Ctrl Pts',(6.53646263654931,-2.08380764381274,9.74946649348901));
#20219=CARTESIAN_POINT('Ctrl Pts',(7.62707430687696,0.0781684385926071,
9.87629376699721));
#20220=CARTESIAN_POINT('Ctrl Pts',(6.40524019402461,2.16878936101054,10.0031210405055));
#20221=CARTESIAN_POINT('Ctrl Pts',(3.98629764241174,2.27965562533786,10.1299483140136));
#20222=CARTESIAN_POINT('Ctrl Pts',(2.57835077524251,0.309564270493552,10.2567755875219));
#20223=CARTESIAN_POINT('Ctrl Pts',(3.46662785364894,-1.94310935489986,10.3836028610301));
#20224=CARTESIAN_POINT('Ctrl Pts',(5.8402752452588,-2.42203765258933,10.5104301345384));
#20225=CARTESIAN_POINT('Ctrl Pts',(7.53253604322313,-0.690036692809079,
10.6372574080466));
#20226=CARTESIAN_POINT('Ctrl Pts',(6.99864916851293,1.67185677837162,10.7640846815548));
#20227=CARTESIAN_POINT('Ctrl Pts',(4.72596736298847,2.50761411959545,10.890911955063));
#20228=CARTESIAN_POINT('Ctrl Pts',(2.78908193177085,1.05432589032441,11.0177392285712));
#20229=CARTESIAN_POINT('Ctrl Pts',(2.95605736637601,-1.36139435666112,11.1445665020794));
#20230=CARTESIAN_POINT('Ctrl Pts',(5.07447069780861,-2.53437624037689,11.2713937755877));
#20231=CARTESIAN_POINT('Ctrl Pts',(7.21055503371717,-1.39389127751139,11.3982210490959));
#20232=CARTESIAN_POINT('Ctrl Pts',(7.41440525221706,1.0190097554844,11.5250483226041));
#20233=CARTESIAN_POINT('Ctrl Pts',(5.49994831735453,2.50168447396085,11.6518755961123));
#20234=CARTESIAN_POINT('Ctrl Pts',(3.21475667759305,1.70079147817141,11.7787028696205));
#20235=CARTESIAN_POINT('Ctrl Pts',(2.6448752597056,-0.652776187180628,11.9055301431287));
#20236=CARTESIAN_POINT('Ctrl Pts',(4.31044945004781,-2.41022346133601,12.0323574166369));
#20237=CARTESIAN_POINT('Ctrl Pts',(6.69120145502419,-1.96798503729974,12.1591846901452));
#20238=CARTESIAN_POINT('Ctrl Pts',(7.61365537643526,0.27158148394315,12.2860119636534));
#20239=CARTESIAN_POINT('Ctrl Pts',(6.23620456203093,2.26156657370656,12.4128392371616));
#20240=CARTESIAN_POINT('Ctrl Pts',(3.81539217578921,2.19032332898847,12.5396665106698));
#20241=CARTESIAN_POINT('Ctrl Pts',(2.56246950519383,0.112970955883516,12.666511084726));
#20242=CARTESIAN_POINT('Ctrl Pts',(3.2667393782928,-1.3312722795269,12.7510799009463));
#20243=CARTESIAN_POINT('Ctrl Pts',(3.84657573841683,-1.74555482053124,12.7933729593303));
#20244=CARTESIAN_POINT('Ctrl Pts',(6.10267445645391,-2.06639516034963,-5.38080962817601));
#20245=CARTESIAN_POINT('Ctrl Pts',(6.78878589364418,-1.73142453862302,-5.33853387033994));
#20246=CARTESIAN_POINT('Ctrl Pts',(7.78943442039165,-0.330311435859617,
-5.25398235466779));
#20247=CARTESIAN_POINT('Ctrl Pts',(6.83455580035441,2.08788418058241,-5.12715508115958));
#20248=CARTESIAN_POINT('Ctrl Pts',(4.28841652026521,2.59358650081123,-5.00032780765136));
#20249=CARTESIAN_POINT('Ctrl Pts',(2.47864613481591,0.73506451413552,-4.87350053414315));
#20250=CARTESIAN_POINT('Ctrl Pts',(3.05550841781776,-1.79616751049385,-4.74667326063492));
#20251=CARTESIAN_POINT('Ctrl Pts',(5.49334425510517,-2.6868904399228,-4.61984598712671));
#20252=CARTESIAN_POINT('Ctrl Pts',(7.56631881088614,-1.12538726028821,-4.49301871361849));
#20253=CARTESIAN_POINT('Ctrl Pts',(7.38239502698786,1.46366017885112,-4.36619144011028));
#20254=CARTESIAN_POINT('Ctrl Pts',(5.10933222983235,2.71649227696918,-4.23936416660206));
#20255=CARTESIAN_POINT('Ctrl Pts',(2.82213990955064,1.48967352577638,-4.11253689309384));
#20256=CARTESIAN_POINT('Ctrl Pts',(2.60861873800462,-1.0970124992201,-3.98570961958563));
#20257=CARTESIAN_POINT('Ctrl Pts',(4.66369838100526,-2.68228438855176,-3.85888234607741));
#20258=CARTESIAN_POINT('Ctrl Pts',(7.11141268456692,-1.81907341315463,-3.7320550725692));
#20259=CARTESIAN_POINT('Ctrl Pts',(7.71739887022894,0.704663164986982,-3.60522779906098));
#20260=CARTESIAN_POINT('Ctrl Pts',(5.92848656513453,2.58515328936164,-3.47840052555276));
#20261=CARTESIAN_POINT('Ctrl Pts',(3.37766543800594,2.10581713208477,-3.35157325204455));
#20262=CARTESIAN_POINT('Ctrl Pts',(2.39342270461766,-0.295790935536472,
-3.22474597853633));
#20263=CARTESIAN_POINT('Ctrl Pts',(3.87421352712319,-2.42738922675253,-3.09791870502811));
#20264=CARTESIAN_POINT('Ctrl Pts',(6.46831467300135,-2.34317314223929,-2.9710914315199));
#20265=CARTESIAN_POINT('Ctrl Pts',(7.80773059670882,-0.12001805996294,-2.84426415801168));
#20266=CARTESIAN_POINT('Ctrl Pts',(6.66979068393416,2.21269408321409,-2.71743688450346));
#20267=CARTESIAN_POINT('Ctrl Pts',(4.09325044158931,2.5255736883019,-2.59060961099524));
#20268=CARTESIAN_POINT('Ctrl Pts',(2.43007523983111,0.533012129272175,-2.46378233748703));
#20269=CARTESIAN_POINT('Ctrl Pts',(3.19847560893134,-1.94610346710782,-2.33695506397881));
#20270=CARTESIAN_POINT('Ctrl Pts',(5.69702602770357,-2.64874070449948,-2.2101277904706));
#20271=CARTESIAN_POINT('Ctrl Pts',(7.64495323354044,-0.933505184612618,
-2.08330051696238));
#20272=CARTESIAN_POINT('Ctrl Pts',(7.26411408280514,1.63386989938877,-1.95647324345417));
#20273=CARTESIAN_POINT('Ctrl Pts',(4.90215325311397,2.70978547336718,-1.82964596994594));
#20274=CARTESIAN_POINT('Ctrl Pts',(2.71515975986988,1.31210427068896,-1.70281869643773));
#20275=CARTESIAN_POINT('Ctrl Pts',(2.69950568063724,-1.28331635661013,-1.57599142292951));
#20276=CARTESIAN_POINT('Ctrl Pts',(4.86948066308565,-2.70727627837548,-1.4491641494213));
#20277=CARTESIAN_POINT('Ctrl Pts',(7.2442477834359,-1.6599299138067,-1.32233687591308));
#20278=CARTESIAN_POINT('Ctrl Pts',(7.65602794949304,0.9026645484479,-1.19550960240486));
#20279=CARTESIAN_POINT('Ctrl Pts',(5.72893233120405,2.64127196853383,-1.06868232889665));
#20280=CARTESIAN_POINT('Ctrl Pts',(3.22208819377429,1.96882438407996,-0.941855055388429));
#20281=CARTESIAN_POINT('Ctrl Pts',(2.42383962866776,-0.50084209370429,-0.815027781880213));
#20282=CARTESIAN_POINT('Ctrl Pts',(4.06285873807033,-2.51332057612591,-0.688200508371996));
#20283=CARTESIAN_POINT('Ctrl Pts',(6.64298561367803,-2.23154302385742,-0.561373234863779));
#20284=CARTESIAN_POINT('Ctrl Pts',(7.80898085194752,0.0872731369294008,
-0.434545961355562));
#20285=CARTESIAN_POINT('Ctrl Pts',(6.49647899260744,2.32642300963191,-0.307718687847347));
#20286=CARTESIAN_POINT('Ctrl Pts',(3.90358239471807,2.44192416048487,-0.18089141433913));
#20287=CARTESIAN_POINT('Ctrl Pts',(2.3971871572253,0.328342680708558,-0.0540641408309133));
#20288=CARTESIAN_POINT('Ctrl Pts',(3.3523889989458,-2.08496267186669,0.0727631326773033));
#20289=CARTESIAN_POINT('Ctrl Pts',(5.89724280848781,-2.59503361914173,0.199590406185519));
#20290=CARTESIAN_POINT('Ctrl Pts',(7.70870779853437,-0.736257711983984,
0.326417679693737));
#20291=CARTESIAN_POINT('Ctrl Pts',(7.13320880461186,1.79460265381826,0.453244953201953));
#20292=CARTESIAN_POINT('Ctrl Pts',(4.69608352231956,2.68728044653302,0.580072226710167));
#20293=CARTESIAN_POINT('Ctrl Pts',(2.62203398103853,1.12690492009508,0.706899500218388));
#20294=CARTESIAN_POINT('Ctrl Pts',(2.80433265922951,-1.46215291532002,0.8337267737266));
#20295=CARTESIAN_POINT('Ctrl Pts',(5.07657028681036,-2.71650113132714,0.960554047234819));
#20296=CARTESIAN_POINT('Ctrl Pts',(7.36456065019403,-1.49112225919901,1.08738132074303));
#20297=CARTESIAN_POINT('Ctrl Pts',(7.5797378305056,1.0954105676307,1.21420859425125));
#20298=CARTESIAN_POINT('Ctrl Pts',(5.52567979183511,2.68201034607753,1.34103586775946));
#20299=CARTESIAN_POINT('Ctrl Pts',(3.07740999739923,1.82036755649042,1.46786314126768));
#20300=CARTESIAN_POINT('Ctrl Pts',(2.46980361743582,-0.70297700385448,1.5946904147759));
#20301=CARTESIAN_POINT('Ctrl Pts',(4.25750720884985,-2.58461702055266,1.72151768828412));
#20302=CARTESIAN_POINT('Ctrl Pts',(6.80863592901645,-2.10691885608516,1.84834496179233));
#20303=CARTESIAN_POINT('Ctrl Pts',(7.79442100999245,0.294056166133873,1.97517223530055));
#20304=CARTESIAN_POINT('Ctrl Pts',(6.31499977909728,2.42660536949851,2.10199950880876));
#20305=CARTESIAN_POINT('Ctrl Pts',(3.7208450407435,2.34405552594312,2.22882678231698));
#20306=CARTESIAN_POINT('Ctrl Pts',(2.38000137305629,0.121761319043953,2.3556540558252));
#20307=CARTESIAN_POINT('Ctrl Pts',(3.51644263173374,-2.21168131979895,2.48248132933342));
#20308=CARTESIAN_POINT('Ctrl Pts',(6.09278136984322,-2.52621588023851,2.60930860284163));
#20309=CARTESIAN_POINT('Ctrl Pts',(7.75723614197039,-0.534723074643263,
2.73613587634985));
#20310=CARTESIAN_POINT('Ctrl Pts',(6.99042838507253,1.94488559350494,2.86296314985806));
#20311=CARTESIAN_POINT('Ctrl Pts',(4.49232981800657,2.64912762038029,2.98979042336628));
#20312=CARTESIAN_POINT('Ctrl Pts',(2.54330123803048,0.935143700493388,3.1166176968745));
#20313=CARTESIAN_POINT('Ctrl Pts',(2.92249116438501,-1.63247548523992,3.24344497038271));
#20314=CARTESIAN_POINT('Ctrl Pts',(5.2837603957697,-2.70990803538419,3.37027224389094));
#20315=CARTESIAN_POINT('Ctrl Pts',(7.47165123407409,-1.31363192985983,3.49709951739914));
#20316=CARTESIAN_POINT('Ctrl Pts',(7.48897247070264,1.28177810671553,3.62392679090736));
#20317=CARTESIAN_POINT('Ctrl Pts',(5.31991261227054,2.70713161154618,3.75075406441558));
#20318=CARTESIAN_POINT('Ctrl Pts',(2.94447322208036,1.66131088755599,3.8775813379238));
#20319=CARTESIAN_POINT('Ctrl Pts',(2.53104706616061,-0.901018540288114,
4.00440861143202));
#20320=CARTESIAN_POINT('Ctrl Pts',(4.45702549765863,-2.64086346573374,4.13123588494022));
#20321=CARTESIAN_POINT('Ctrl Pts',(6.96430106258761,-1.97002628377034,4.25806315844845));
#20322=CARTESIAN_POINT('Ctrl Pts',(7.7641358458131,0.499126931957104,4.38489043195666));
#20323=CARTESIAN_POINT('Ctrl Pts',(6.12640978402113,2.51265781816716,4.51171770546489));
#20324=CARTESIAN_POINT('Ctrl Pts',(3.54610244174684,2.23253766073493,4.63854497897309));
#20325=CARTESIAN_POINT('Ctrl Pts',(2.37861795947216,-0.0855290481503543,
4.76537225248131));
#20326=CARTESIAN_POINT('Ctrl Pts',(3.68968123688074,-2.32552154050947,4.89219952598953));
#20327=CARTESIAN_POINT('Ctrl Pts',(6.28250310802764,-2.44268820683033,5.01902679949774));
#20328=CARTESIAN_POINT('Ctrl Pts',(7.79025568742204,-0.330074791525955,
5.14585407300597));
#20329=CARTESIAN_POINT('Ctrl Pts',(6.83660422216671,2.08384363418999,5.27268134651417));
#20330=CARTESIAN_POINT('Ctrl Pts',(4.29207858017239,2.59554915539126,5.39950862002241));
#20331=CARTESIAN_POINT('Ctrl Pts',(2.47941998475138,0.737937220771773,5.5263358935306));
#20332=CARTESIAN_POINT('Ctrl Pts',(3.05329316943561,-1.79329229294183,5.65316316703884));
#20333=CARTESIAN_POINT('Ctrl Pts',(5.4898445400539,-2.68753538155518,5.77999044054704));
#20334=CARTESIAN_POINT('Ctrl Pts',(7.56489595595383,-1.12849243648723,5.90681771405526));
#20335=CARTESIAN_POINT('Ctrl Pts',(7.38426038885078,1.46068196379789,6.03364498756347));
#20336=CARTESIAN_POINT('Ctrl Pts',(5.11282895683061,2.71648948600237,6.1604722610717));
#20337=CARTESIAN_POINT('Ctrl Pts',(2.8240519470539,1.49258055037353,6.28729953457991));
#20338=CARTESIAN_POINT('Ctrl Pts',(2.60721335958723,-1.09381352443021,6.41412680808813));
#20339=CARTESIAN_POINT('Ctrl Pts',(4.66025182692117,-2.68173239352949,6.54095408159633));
#20340=CARTESIAN_POINT('Ctrl Pts',(7.10907458990993,-1.8216624204095,6.66778135510457));
#20341=CARTESIAN_POINT('Ctrl Pts',(7.7183017072763,0.701291325234671,6.79460862861277));
#20342=CARTESIAN_POINT('Ctrl Pts',(5.93180715045433,2.58407927974254,6.921435902121));
#20343=CARTESIAN_POINT('Ctrl Pts',(3.38037210862516,2.10801992365272,7.04826317562921));
#20344=CARTESIAN_POINT('Ctrl Pts',(2.3930449719694,-0.292321387164904,7.17509044913742));
#20345=CARTESIAN_POINT('Ctrl Pts',(3.87109606111463,-2.42582045233252,7.30191772264565));
#20346=CARTESIAN_POINT('Ctrl Pts',(6.46530328992434,-2.34493697326663,7.42874499615385));
#20347=CARTESIAN_POINT('Ctrl Pts',(7.8075741649591,-0.123504511716634,7.55557226966209));
#20348=CARTESIAN_POINT('Ctrl Pts',(6.67263202056451,2.21066763533496,7.68239954317029));
#20349=CARTESIAN_POINT('Ctrl Pts',(4.09649585429084,2.52685703428968,7.80922681667851));
#20350=CARTESIAN_POINT('Ctrl Pts',(2.43076219616156,0.536433797043339,7.93605409018673));
#20351=CARTESIAN_POINT('Ctrl Pts',(3.19597702572634,-1.94366691619542,8.06288136369493));
#20352=CARTESIAN_POINT('Ctrl Pts',(5.69362270968416,-2.64951344385026,8.18970863720316));
#20353=CARTESIAN_POINT('Ctrl Pts',(7.64375185995891,-0.936781830185868,
8.31653591071137));
#20354=CARTESIAN_POINT('Ctrl Pts',(7.26621131426039,1.63108039733716,8.4433631842196));
#20355=CARTESIAN_POINT('Ctrl Pts',(4.90563465555995,2.71002947936219,8.5701904577278));
#20356=CARTESIAN_POINT('Ctrl Pts',(2.716847374891,1.31515904696063,8.69701773123603));
#20357=CARTESIAN_POINT('Ctrl Pts',(2.69785898803786,-1.28023932791378,8.82384500474423));
#20358=CARTESIAN_POINT('Ctrl Pts',(4.86600282746846,-2.70698582775575,8.95067227825246));
#20359=CARTESIAN_POINT('Ctrl Pts',(7.24211350736936,-1.66269117579839,9.07749955176067));
#20360=CARTESIAN_POINT('Ctrl Pts',(7.65718548257792,0.899372160304488,9.20432682526889));
#20361=CARTESIAN_POINT('Ctrl Pts',(5.73232503252422,2.64045387338719,9.33115409877711));
#20362=CARTESIAN_POINT('Ctrl Pts',(3.22461907467068,1.97122737042217,9.45798137228532));
#20363=CARTESIAN_POINT('Ctrl Pts',(2.42319840325199,-0.497411563911216,
9.58480864579354));
#20364=CARTESIAN_POINT('Ctrl Pts',(4.05963074187124,-2.51199402413522,9.71163591930176));
#20365=CARTESIAN_POINT('Ctrl Pts',(6.64011748580997,-2.23353137516274,9.83846319280997));
#20366=CARTESIAN_POINT('Ctrl Pts',(7.80909073102681,0.0837849216372962,
9.96529046631819));
#20367=CARTESIAN_POINT('Ctrl Pts',(6.49946657526425,2.32461911650972,10.0921177398264));
#20368=CARTESIAN_POINT('Ctrl Pts',(3.90672050305093,2.44345123643088,10.2189450133346));
#20369=CARTESIAN_POINT('Ctrl Pts',(2.39761119935786,0.331806783044349,10.3457722868428));
#20370=CARTESIAN_POINT('Ctrl Pts',(3.34971190325417,-2.08272376887925,10.472599560351));
#20371=CARTESIAN_POINT('Ctrl Pts',(5.89390831143774,-2.59606355939153,10.5994268338592));
#20372=CARTESIAN_POINT('Ctrl Pts',(7.70775979549099,-0.739616541852521,
10.7262541073675));
#20373=CARTESIAN_POINT('Ctrl Pts',(7.13551259743823,1.79198141457968,10.8530813808757));
#20374=CARTESIAN_POINT('Ctrl Pts',(4.69953625697684,2.68778878393482,10.9799086543839));
#20375=CARTESIAN_POINT('Ctrl Pts',(2.62348360712445,1.13008029444468,11.1067359278921));
#20376=CARTESIAN_POINT('Ctrl Pts',(2.80245639915702,-1.45921194722585,11.2335632014003));
#20377=CARTESIAN_POINT('Ctrl Pts',(5.07307991633565,-2.71647379073412,11.3603904749085));
#20378=CARTESIAN_POINT('Ctrl Pts',(7.36264411791226,-1.49404380540182,11.4872177484168));
#20379=CARTESIAN_POINT('Ctrl Pts',(7.5811411851465,1.09222665884215,11.614045021925));
#20380=CARTESIAN_POINT('Ctrl Pts',(5.52912854227627,2.68143308713726,11.7408722954332));
#20381=CARTESIAN_POINT('Ctrl Pts',(3.07974352306788,1.82299510244365,11.8676995689414));
#20382=CARTESIAN_POINT('Ctrl Pts',(2.46891553673564,-0.699678830412259,
11.9945268424496));
#20383=CARTESIAN_POINT('Ctrl Pts',(4.25416295284739,-2.58340050629504,12.1213541159578));
#20384=CARTESIAN_POINT('Ctrl Pts',(6.80597444820543,-2.109386794751,12.2481813894661));
#20385=CARTESIAN_POINT('Ctrl Pts',(7.7947076365739,0.291094894051927,12.3750086629743));
#20386=CARTESIAN_POINT('Ctrl Pts',(6.318285558533,2.42406246775762,12.5018359364825));
#20387=CARTESIAN_POINT('Ctrl Pts',(3.72353530214159,2.34770032232699,12.6286632099907));
#20388=CARTESIAN_POINT('Ctrl Pts',(2.38058884365411,0.121088035739373,12.755507784047));
#20389=CARTESIAN_POINT('Ctrl Pts',(3.13546123450027,-1.42692556773965,12.8400766002673));
#20390=CARTESIAN_POINT('Ctrl Pts',(3.75695943595017,-1.87097473718329,12.8823696586513));
#20391=CARTESIAN_POINT('Ctrl Pts',(6.17030206354638,-2.20491499369139,-5.29181292885504));
#20392=CARTESIAN_POINT('Ctrl Pts',(6.90240666010767,-1.84748977296731,-5.24953717101897));
#20393=CARTESIAN_POINT('Ctrl Pts',(7.97013319294923,-0.352453708511098,
-5.16498565534682));
#20394=CARTESIAN_POINT('Ctrl Pts',(6.95124473111254,2.22784452034734,-5.0381583818386));
#20395=CARTESIAN_POINT('Ctrl Pts',(4.23442619493992,2.76744635914975,-4.91133110833039));
#20396=CARTESIAN_POINT('Ctrl Pts',(2.3033386979383,0.784339220129447,-4.78450383482217));
#20397=CARTESIAN_POINT('Ctrl Pts',(2.91887067434431,-1.91657275968413,-4.65767656131396));
#20398=CARTESIAN_POINT('Ctrl Pts',(5.52012569706886,-2.86700488419138,-4.53084928780574));
#20399=CARTESIAN_POINT('Ctrl Pts',(7.73206113288786,-1.20082706905823,-4.40402201429753));
#20400=CARTESIAN_POINT('Ctrl Pts',(7.53580810413746,1.56177595454288,-4.2771947407893));
#20401=CARTESIAN_POINT('Ctrl Pts',(5.11037160524329,2.89859106654255,-4.1503674672811));
#20402=CARTESIAN_POINT('Ctrl Pts',(2.66985841724704,1.58953309401564,-4.02354019377287));
#20403=CARTESIAN_POINT('Ctrl Pts',(2.44202395380747,-1.17055021914974,-3.89671292026466));
#20404=CARTESIAN_POINT('Ctrl Pts',(4.63486489973541,-2.86209006832044,-3.76988564675644));
#20405=CARTESIAN_POINT('Ctrl Pts',(7.24666058710183,-1.94101414881913,-3.64305837324822));
#20406=CARTESIAN_POINT('Ctrl Pts',(7.89326877336469,0.75189993075619,-3.51623109974001));
#20407=CARTESIAN_POINT('Ctrl Pts',(5.98443756838148,2.75844783131394,-3.38940382623179));
#20408=CARTESIAN_POINT('Ctrl Pts',(3.26262333974239,2.24697959886835,-3.26257655272358));
#20409=CARTESIAN_POINT('Ctrl Pts',(2.21240235494661,-0.315619142590331,
-3.13574927921536));
#20410=CARTESIAN_POINT('Ctrl Pts',(3.79245729783111,-2.59010812853723,-3.00892200570714));
#20411=CARTESIAN_POINT('Ctrl Pts',(6.56045280103919,-2.50024665817753,-2.88209473219892));
#20412=CARTESIAN_POINT('Ctrl Pts',(7.98965584489067,-0.128063414492935,
-2.75526745869071));
#20413=CARTESIAN_POINT('Ctrl Pts',(6.77543466215609,2.36102099644168,-2.62844018518249));
#20414=CARTESIAN_POINT('Ctrl Pts',(4.0261772494383,2.6948743395562,-2.50161291167428));
#20415=CARTESIAN_POINT('Ctrl Pts',(2.25151187571962,0.568742348125107,-2.37478563816606));
#20416=CARTESIAN_POINT('Ctrl Pts',(3.07142160426369,-2.07655960304068,-2.24795836465784));
#20417=CARTESIAN_POINT('Ctrl Pts',(5.7374611820532,-2.8262977990925,-2.12113109114962));
#20418=CARTESIAN_POINT('Ctrl Pts',(7.81596677729586,-0.996082268162477,
-1.99430381764141));
#20419=CARTESIAN_POINT('Ctrl Pts',(7.40959825216883,1.74339560410787,-1.86747654413319));
#20420=CARTESIAN_POINT('Ctrl Pts',(4.88930448269607,2.89143467549714,-1.74064927062498));
#20421=CARTESIAN_POINT('Ctrl Pts',(2.55570690325562,1.4000605669436,-1.61382199711676));
#20422=CARTESIAN_POINT('Ctrl Pts',(2.53900346014134,-1.3693428685055,-1.48699472360854));
#20423=CARTESIAN_POINT('Ctrl Pts',(4.85444170087268,-2.88875727779245,-1.36016745010033));
#20424=CARTESIAN_POINT('Ctrl Pts',(7.38840022471071,-1.77120253940683,-1.23334017659211));
#20425=CARTESIAN_POINT('Ctrl Pts',(7.8277838816539,0.963174244373312,-1.10651290308389));
#20426=CARTESIAN_POINT('Ctrl Pts',(5.77150630968967,2.81832839990373,-0.979685629575677));
#20427=CARTESIAN_POINT('Ctrl Pts',(3.09661704769054,2.10080360605791,-0.852858356067459));
#20428=CARTESIAN_POINT('Ctrl Pts',(2.24485826327766,-0.534415809265402,
-0.726031082559243));
#20429=CARTESIAN_POINT('Ctrl Pts',(3.99374825228489,-2.68179984573495,-0.599203809051027));
#20430=CARTESIAN_POINT('Ctrl Pts',(6.74683272654919,-2.3811334670074,-0.47237653554281));
#20431=CARTESIAN_POINT('Ctrl Pts',(7.99098991040469,0.0931234508551305,
-0.345549262034593));
#20432=CARTESIAN_POINT('Ctrl Pts',(6.59050510264064,2.48237368826305,-0.218721988526377));
#20433=CARTESIAN_POINT('Ctrl Pts',(3.82379489373254,2.60561740475589,-0.0918947150181613));
#20434=CARTESIAN_POINT('Ctrl Pts',(2.21641915587456,0.350352978779065,0.0349325584900565));
#20435=CARTESIAN_POINT('Ctrl Pts',(3.23565250640894,-2.22472716966094,0.161759831998273));
#20436=CARTESIAN_POINT('Ctrl Pts',(5.9510994011173,-2.76899048438087,0.288587105506489));
#20437=CARTESIAN_POINT('Ctrl Pts',(7.88399509974297,-0.785612403437753,
0.415414379014706));
#20438=CARTESIAN_POINT('Ctrl Pts',(7.26991779986226,1.91490300357299,0.542241652522922));
#20439=CARTESIAN_POINT('Ctrl Pts',(4.66942096385466,2.86742103471235,0.669068926031139));
#20440=CARTESIAN_POINT('Ctrl Pts',(2.45633848138528,1.2024464644806,0.795896199539355));
#20441=CARTESIAN_POINT('Ctrl Pts',(2.65085746622716,-1.56016765230576,0.922723473047572));
#20442=CARTESIAN_POINT('Ctrl Pts',(5.07541348069008,-2.89860051444825,1.04955074655579));
#20443=CARTESIAN_POINT('Ctrl Pts',(7.51677820823447,-1.59107894260581,1.176378020064));
#20444=CARTESIAN_POINT('Ctrl Pts',(7.74637969021288,1.16884090282531,1.30320529357222));
#20445=CARTESIAN_POINT('Ctrl Pts',(5.55462883138362,2.86179765553708,1.43003256708044));
#20446=CARTESIAN_POINT('Ctrl Pts',(2.94224041607201,1.94239504444831,1.55685984058865));
#20447=CARTESIAN_POINT('Ctrl Pts',(2.29390342654034,-0.750100738600607,
1.68368711409687));
#20448=CARTESIAN_POINT('Ctrl Pts',(4.20144489228679,-2.75787561397612,1.81051438760508));
#20449=CARTESIAN_POINT('Ctrl Pts',(6.92358733331937,-2.24815517642194,1.93734166111331));
#20450=CARTESIAN_POINT('Ctrl Pts',(7.97545405625221,0.313768083731995,2.06416893462152));
#20451=CARTESIAN_POINT('Ctrl Pts',(6.39686051491129,2.58927172577871,2.19099620812974));
#20452=CARTESIAN_POINT('Ctrl Pts',(3.62880782668101,2.50118819206035,2.31782348163795));
#20453=CARTESIAN_POINT('Ctrl Pts',(2.19808133069975,0.129923532131306,2.44465075514617));
#20454=CARTESIAN_POINT('Ctrl Pts',(3.41070339776045,-2.35994034290457,2.57147802865439));
#20455=CARTESIAN_POINT('Ctrl Pts',(6.15974579850069,-2.69555958052898,2.6983053021626));
#20456=CARTESIAN_POINT('Ctrl Pts',(7.93577651798969,-0.570567985919117,
2.82513257567082));
#20457=CARTESIAN_POINT('Ctrl Pts',(7.11756616166227,2.0752600898503,2.95195984917904));
#20458=CARTESIAN_POINT('Ctrl Pts',(4.4520087252469,2.82671065169848,3.07878712268725));
#20459=CARTESIAN_POINT('Ctrl Pts',(2.37232792576459,0.997830621189154,3.20561439619547));
#20460=CARTESIAN_POINT('Ctrl Pts',(2.77693667152565,-1.74190771605857,3.33244166970368));
#20461=CARTESIAN_POINT('Ctrl Pts',(5.29649248172284,-2.89156545340167,3.45926894321191));
#20462=CARTESIAN_POINT('Ctrl Pts',(7.63104755933012,-1.40169063203266,3.58609621672012));
#20463=CARTESIAN_POINT('Ctrl Pts',(7.64952991695677,1.3677015027485,3.71292349022833));
#20464=CARTESIAN_POINT('Ctrl Pts',(5.33506814515229,2.88860291328989,3.83975076373655));
#20465=CARTESIAN_POINT('Ctrl Pts',(2.80039228617996,1.77267608608568,3.96657803724477));
#20466=CARTESIAN_POINT('Ctrl Pts',(2.35925230121338,-0.961417896826199,
4.09340531075299));
#20467=CARTESIAN_POINT('Ctrl Pts',(4.41433779629248,-2.81789251330945,4.2202325842612));
#20468=CARTESIAN_POINT('Ctrl Pts',(7.08968740633153,-2.10208607453204,4.34705985776942));
#20469=CARTESIAN_POINT('Ctrl Pts',(7.94313874025325,0.532585672452493,4.47388713127763));
#20470=CARTESIAN_POINT('Ctrl Pts',(6.1956284776986,2.68109266010633,4.60071440478585));
#20471=CARTESIAN_POINT('Ctrl Pts',(3.44235143926906,2.38219477890292,4.72754167829407));
#20472=CARTESIAN_POINT('Ctrl Pts',(2.19660518063288,-0.0912624479003074,
4.85436895180227));
#20473=CARTESIAN_POINT('Ctrl Pts',(3.59555497179828,-2.48141178957951,4.98119622531051));
#20474=CARTESIAN_POINT('Ctrl Pts',(6.3621854446917,-2.60643266859086,5.10802349881871));
#20475=CARTESIAN_POINT('Ctrl Pts',(7.97100951323098,-0.352201200835182,
5.23485077232694));
#20476=CARTESIAN_POINT('Ctrl Pts',(6.95343046792319,2.22353311781684,5.36167804583515));
#20477=CARTESIAN_POINT('Ctrl Pts',(4.23833373932061,2.76954057936184,5.48850531934335));
#20478=CARTESIAN_POINT('Ctrl Pts',(2.30416442254237,0.787404497311804,5.61533259285159));
#20479=CARTESIAN_POINT('Ctrl Pts',(2.9165069278227,-1.91350480326794,5.74215986635979));
#20480=CARTESIAN_POINT('Ctrl Pts',(5.51639138025557,-2.86769305918452,5.86898713986803));
#20481=CARTESIAN_POINT('Ctrl Pts',(7.73054289754047,-1.20414039929179,5.99581441337622));
#20482=CARTESIAN_POINT('Ctrl Pts',(7.53779850966063,1.55859809623616,6.12264168688445));
#20483=CARTESIAN_POINT('Ctrl Pts',(5.11410273370085,2.89858808848458,6.24946896039267));
#20484=CARTESIAN_POINT('Ctrl Pts',(2.67189862729027,1.59263498964734,6.37629623390088));
#20485=CARTESIAN_POINT('Ctrl Pts',(2.44052436650502,-1.16713680258064,6.5031235074091));
#20486=CARTESIAN_POINT('Ctrl Pts',(4.63118730750988,-2.86150107056997,6.6299507809173));
#20487=CARTESIAN_POINT('Ctrl Pts',(7.24416575936279,-1.94377670896474,6.75677805442554));
#20488=CARTESIAN_POINT('Ctrl Pts',(7.89423213167136,0.748302061302728,6.88360532793373));
#20489=CARTESIAN_POINT('Ctrl Pts',(5.98798074758552,2.75730182596224,7.01043260144197));
#20490=CARTESIAN_POINT('Ctrl Pts',(3.26551145076094,2.24933005353904,7.13725987495017));
#20491=CARTESIAN_POINT('Ctrl Pts',(2.21199930116691,-0.311917014666013,
7.2640871484584));
#20492=CARTESIAN_POINT('Ctrl Pts',(3.78913085394635,-2.58843419205753,7.39091442196661));
#20493=CARTESIAN_POINT('Ctrl Pts',(6.55723955130574,-2.50212872679302,7.51774169547482));
#20494=CARTESIAN_POINT('Ctrl Pts',(7.98948892681172,-0.131783578909695,
7.64456896898306));
#20495=CARTESIAN_POINT('Ctrl Pts',(6.77846646645888,2.35885870657652,7.77139624249124));
#20496=CARTESIAN_POINT('Ctrl Pts',(4.02964021686276,2.69624371404217,7.8982235159995));
#20497=CARTESIAN_POINT('Ctrl Pts',(2.25224488184646,0.57239338579536,8.02505078950768));
#20498=CARTESIAN_POINT('Ctrl Pts',(3.06875552970189,-2.07395971907718,8.15187806301592));
#20499=CARTESIAN_POINT('Ctrl Pts',(5.73382972420172,-2.82712233866435,8.27870533652413));
#20500=CARTESIAN_POINT('Ctrl Pts',(7.81468487019807,-0.999578562139587,
8.40553261003235));
#20501=CARTESIAN_POINT('Ctrl Pts',(7.41183607055402,1.74041910909059,8.53235988354056));
#20502=CARTESIAN_POINT('Ctrl Pts',(4.89301925932717,2.89169503831994,8.65918715704877));
#20503=CARTESIAN_POINT('Ctrl Pts',(2.55750764676054,1.40332011871425,8.786014430557));
#20504=CARTESIAN_POINT('Ctrl Pts',(2.53724638227356,-1.3660595726293,8.91284170406521));
#20505=CARTESIAN_POINT('Ctrl Pts',(4.8507307301711,-2.88844735695125,9.03966897757343));
#20506=CARTESIAN_POINT('Ctrl Pts',(7.38612287844602,-1.77414890130498,9.16649625108164));
#20507=CARTESIAN_POINT('Ctrl Pts',(7.82901900942787,0.959661152530205,9.29332352458986));
#20508=CARTESIAN_POINT('Ctrl Pts',(5.77512643915643,2.81745546413148,9.42015079809808));
#20509=CARTESIAN_POINT('Ctrl Pts',(3.09931758500439,2.10336767546596,9.54697807160629));
#20510=CARTESIAN_POINT('Ctrl Pts',(2.24417405361598,-0.530755315511743,
9.67380534511451));
#20511=CARTESIAN_POINT('Ctrl Pts',(3.99030386886996,-2.68038436895184,9.80063261862273));
#20512=CARTESIAN_POINT('Ctrl Pts',(6.74377233507061,-2.38325510651274,9.92745989213094));
#20513=CARTESIAN_POINT('Ctrl Pts',(7.99110715517667,0.0894014046819865,
10.0542871656391));
#20514=CARTESIAN_POINT('Ctrl Pts',(6.59369295650387,2.48044887200891,10.1811144391474));
#20515=CARTESIAN_POINT('Ctrl Pts',(3.82714336369014,2.60724684752389,10.3079417126556));
#20516=CARTESIAN_POINT('Ctrl Pts',(2.2168716234732,0.354049295595143,10.4347689861638));
#20517=CARTESIAN_POINT('Ctrl Pts',(3.23279595285942,-2.22233818285863,10.561596259672));
#20518=CARTESIAN_POINT('Ctrl Pts',(5.94754137761666,-2.77008946619374,10.6884235331802));
#20519=CARTESIAN_POINT('Ctrl Pts',(7.88298354775886,-0.789196390895958,
10.8152508066884));
#20520=CARTESIAN_POINT('Ctrl Pts',(7.2723760263635,1.91210605078773,10.9420780801967));
#20521=CARTESIAN_POINT('Ctrl Pts',(4.67310515096523,2.86796344827419,11.0689053537049));
#20522=CARTESIAN_POINT('Ctrl Pts',(2.45788528247802,1.20583469856495,11.1957326272131));
#20523=CARTESIAN_POINT('Ctrl Pts',(2.64885543193806,-1.55702953779058,11.3225599007213));
#20524=CARTESIAN_POINT('Ctrl Pts',(5.07168913486267,-2.89857134109138,11.4493871742295));
#20525=CARTESIAN_POINT('Ctrl Pts',(7.51473320210737,-1.59419633329225,11.5762144477377));
#20526=CARTESIAN_POINT('Ctrl Pts',(7.74787711807591,1.16544356219989,11.703041721246));
#20527=CARTESIAN_POINT('Ctrl Pts',(5.558308767198,2.86118170031369,11.8298689947542));
#20528=CARTESIAN_POINT('Ctrl Pts',(2.94473036854272,1.94519872671588,11.9566962682624));
#20529=CARTESIAN_POINT('Ctrl Pts',(2.29295581376568,-0.746581473643887,
12.0835235417706));
#20530=CARTESIAN_POINT('Ctrl Pts',(4.19787645564695,-2.75657755125406,12.2103508152788));
#20531=CARTESIAN_POINT('Ctrl Pts',(6.9207474413867,-2.25078855220226,12.3371780887871));
#20532=CARTESIAN_POINT('Ctrl Pts',(7.97575989671253,0.310608304160704,12.4640053622953));
#20533=CARTESIAN_POINT('Ctrl Pts',(6.40036655503507,2.58655836180867,12.5908326358035));
#20534=CARTESIAN_POINT('Ctrl Pts',(3.63167842849399,2.50507731566553,12.7176599093117));
#20535=CARTESIAN_POINT('Ctrl Pts',(2.19870818211441,0.129205115595229,12.844504483368));
#20536=CARTESIAN_POINT('Ctrl Pts',(3.00418309070775,-1.52257885595242,12.9290732995882));
#20537=CARTESIAN_POINT('Ctrl Pts',(3.66734313348352,-1.99639465383534,12.9713663579723));
#20538=CARTESIAN_POINT('Ctrl Pts',(4.01617654290848,2.20524431464374,12.706362531166));
#20539=CARTESIAN_POINT('Ctrl Pts',(3.96412481280005,2.1740903404473,12.706362531166));
#20540=CARTESIAN_POINT('Ctrl Pts',(3.91342899343042,2.14094354517164,12.706362531166));
#20541=CARTESIAN_POINT('Ctrl Pts',(3.8642154788866,2.10580426985646,12.706362531166));
#20542=CARTESIAN_POINT('Ctrl Pts',(3.7955725456219,2.05679206349834,12.706362531166));
#20543=CARTESIAN_POINT('Ctrl Pts',(3.72981155181425,2.00390483037292,12.706362531166));
#20544=CARTESIAN_POINT('Ctrl Pts',(3.66707598254363,1.94750832456937,12.706362531166));
#20545=CARTESIAN_POINT('Ctrl Pts',(3.60356184354373,1.89041191896788,12.706362531166));
#20546=CARTESIAN_POINT('Ctrl Pts',(3.54314820656414,1.82971763964448,12.706362531166));
#20547=CARTESIAN_POINT('Ctrl Pts',(3.48602767856145,1.76577476703768,12.706362531166));
#20548=CARTESIAN_POINT('Ctrl Pts',(3.43577223874705,1.7095169329767,12.706362531166));
#20549=CARTESIAN_POINT('Ctrl Pts',(3.38806637215777,1.65074357121809,12.706362531166));
#20550=CARTESIAN_POINT('Ctrl Pts',(3.34307309132191,1.58968252285634,12.706362531166));
#20551=CARTESIAN_POINT('Ctrl Pts',(3.33502299263552,1.57875761460171,12.706362531166));
#20552=CARTESIAN_POINT('Ctrl Pts',(3.32705953936463,1.56775894682874,12.706362531166));
#20553=CARTESIAN_POINT('Ctrl Pts',(3.31919274731376,1.55670083255366,12.706362531166));
#20554=CARTESIAN_POINT('Ctrl Pts',(3.27051921520694,1.48828190438977,12.706362531166));
#20555=CARTESIAN_POINT('Ctrl Pts',(3.22545495269274,1.41747248052991,12.706362531166));
#20556=CARTESIAN_POINT('Ctrl Pts',(3.18414803610741,1.34462167953958,12.706362531166));
#20557=CARTESIAN_POINT('Ctrl Pts',(3.14298608776046,1.27202655128295,12.706362531166));
#20558=CARTESIAN_POINT('Ctrl Pts',(3.10555484108553,1.19740334531551,12.706362531166));
#20559=CARTESIAN_POINT('Ctrl Pts',(3.07204921526324,1.12108015481246,12.706362531166));
#20560=CARTESIAN_POINT('Ctrl Pts',(3.0393754946111,1.04665197910837,12.706362531166));
#20561=CARTESIAN_POINT('Ctrl Pts',(3.01043477138293,0.970606298836382,12.706362531166));
#20562=CARTESIAN_POINT('Ctrl Pts',(2.98545673362889,0.893244772984474,12.706362531166));
#20563=CARTESIAN_POINT('Ctrl Pts',(2.97373044481661,0.856926323792001,12.706362531166));
#20564=CARTESIAN_POINT('Ctrl Pts',(2.9628782381547,0.820317910312545,12.706362531166));
#20565=CARTESIAN_POINT('Ctrl Pts',(2.95292784475094,0.783451362266065,12.706362531166));
#20566=CARTESIAN_POINT('Ctrl Pts',(2.94898502933406,0.768843096230084,12.706362531166));
#20567=CARTESIAN_POINT('Ctrl Pts',(2.94518353990657,0.754192671177584,12.706362531166));
#20568=CARTESIAN_POINT('Ctrl Pts',(2.94153002573792,0.739522721976762,12.706362531166));
#20569=CARTESIAN_POINT('Ctrl Pts',(2.92212297738889,0.661597633890026,12.706362531166));
#20570=CARTESIAN_POINT('Ctrl Pts',(2.90685063396446,0.582991787835282,12.706362531166));
#20571=CARTESIAN_POINT('Ctrl Pts',(2.89588468653661,0.504004912306211,12.706362531166));
#20572=CARTESIAN_POINT('Ctrl Pts',(2.88523725179527,0.427312259149472,12.706362531166));
#20573=CARTESIAN_POINT('Ctrl Pts',(2.87864967603292,0.350259608145263,12.706362531166));
#20574=CARTESIAN_POINT('Ctrl Pts',(2.87632731099095,0.273124066218685,12.706362531166));
#20575=CARTESIAN_POINT('Ctrl Pts',(2.87460628536994,0.215961543726355,12.706362531166));
#20576=CARTESIAN_POINT('Ctrl Pts',(2.87522858516988,0.158753502861158,12.706362531166));
#20577=CARTESIAN_POINT('Ctrl Pts',(2.87829576895771,0.101617392022989,12.706362531166));
#20578=CARTESIAN_POINT('Ctrl Pts',(2.88063481507154,0.0580451748816736,
12.706362531166));
#20579=CARTESIAN_POINT('Ctrl Pts',(2.88439617502459,0.0145148557028028,
12.706362531166));
#20580=CARTESIAN_POINT('Ctrl Pts',(2.88955511502261,-0.0289182870924016,
12.706362531166));
#20581=CARTESIAN_POINT('Ctrl Pts',(2.891997784775,-0.0494831364989744,12.706362531166));
#20582=CARTESIAN_POINT('Ctrl Pts',(2.89475382668687,-0.0700261632891898,
12.7063625311661));
#20583=CARTESIAN_POINT('Ctrl Pts',(2.89782089320795,-0.0905412794435463,
12.7063625311661));
#20584=CARTESIAN_POINT('Ctrl Pts',(2.89963471943402,-0.10267367222214,12.706362531166));
#20585=CARTESIAN_POINT('Ctrl Pts',(2.90155583066391,-0.114786297038073,
12.7063625311661));
#20586=CARTESIAN_POINT('Ctrl Pts',(2.90358323488813,-0.126877932230494,
12.706362531166));
#20587=CARTESIAN_POINT('Ctrl Pts',(2.91645442833662,-0.203642976818655,
12.7063625311661));
#20588=CARTESIAN_POINT('Ctrl Pts',(2.93360576650297,-0.279564944346245,
12.7063625311661));
#20589=CARTESIAN_POINT('Ctrl Pts',(2.95481919736294,-0.354355451724281,
12.7063625311661));
#20590=CARTESIAN_POINT('Ctrl Pts',(2.97622105807171,-0.429810291245941,
12.7063625311661));
#20591=CARTESIAN_POINT('Ctrl Pts',(3.00175809900175,-0.504114372604786,
12.7063625311661));
#20592=CARTESIAN_POINT('Ctrl Pts',(3.03125399139832,-0.576948215175514,
12.7063625311661));
#20593=CARTESIAN_POINT('Ctrl Pts',(3.06045458320581,-0.649052875651101,
12.7063625311661));
#20594=CARTESIAN_POINT('Ctrl Pts',(3.09353584953513,-0.719717347631348,
12.7063625311661));
#20595=CARTESIAN_POINT('Ctrl Pts',(3.13036322612031,-0.788596670847388,
12.7063625311661));
#20596=CARTESIAN_POINT('Ctrl Pts',(3.13841107268683,-0.803648794464367,
12.7063625311661));
#20597=CARTESIAN_POINT('Ctrl Pts',(3.14663793160898,-0.818615510215626,
12.7063625311661));
#20598=CARTESIAN_POINT('Ctrl Pts',(3.15504258425979,-0.833492938132457,
12.7063625311661));
#20599=CARTESIAN_POINT('Ctrl Pts',(3.16198740923832,-0.84578626390163,12.7063625311661));
#20600=CARTESIAN_POINT('Ctrl Pts',(3.16905363004956,-0.85801862357911,12.7063625311661));
#20601=CARTESIAN_POINT('Ctrl Pts',(3.17624058869617,-0.870187770193119,
12.7063625311661));
#20602=CARTESIAN_POINT('Ctrl Pts',(3.18310939201618,-0.881818207875329,
12.7063625311661));
#20603=CARTESIAN_POINT('Ctrl Pts',(3.1900833958179,-0.893382290911527,12.7063625311661));
#20604=CARTESIAN_POINT('Ctrl Pts',(3.19716136682681,-0.904877975358936,
12.7063625311661));
#20605=CARTESIAN_POINT('Ctrl Pts',(3.2371698418621,-0.969857727840078,12.7063625311661));
#20606=CARTESIAN_POINT('Ctrl Pts',(3.28050020814543,-1.03265978440192,12.7063625311661));
#20607=CARTESIAN_POINT('Ctrl Pts',(3.3269982826191,-1.09297461243398,12.7063625311661));
#20608=CARTESIAN_POINT('Ctrl Pts',(3.36850332953163,-1.14681275079408,12.7063625311661));
#20609=CARTESIAN_POINT('Ctrl Pts',(3.41253311578195,-1.1986690627602,12.7063625311661));
#20610=CARTESIAN_POINT('Ctrl Pts',(3.45899756854344,-1.2482942239992,12.7063625311661));
#20611=CARTESIAN_POINT('Ctrl Pts',(3.47176322594664,-1.26192825537815,12.7063625311661));
#20612=CARTESIAN_POINT('Ctrl Pts',(3.4847127467252,-1.27539369266552,12.7063625311661));
#20613=CARTESIAN_POINT('Ctrl Pts',(3.49784445064999,-1.28868493357174,12.7063625311661));
#20614=CARTESIAN_POINT('Ctrl Pts',(3.50919570582733,-1.30017409507081,12.7063625311661));
#20615=CARTESIAN_POINT('Ctrl Pts',(3.52068411570671,-1.31153392785575,12.7063625311661));
#20616=CARTESIAN_POINT('Ctrl Pts',(3.53229553060125,-1.32274849072851,12.7063625311661));
#20617=CARTESIAN_POINT('Ctrl Pts',(3.58532462221074,-1.3739651673645,12.7063625311661));
#20618=CARTESIAN_POINT('Ctrl Pts',(3.64097669980664,-1.42221694716149,12.7063625311661));
#20619=CARTESIAN_POINT('Ctrl Pts',(3.69912395167213,-1.4671959866198,12.7063625311661));
#20620=CARTESIAN_POINT('Ctrl Pts',(3.75558706950963,-1.51087228642202,12.7063625311661));
#20621=CARTESIAN_POINT('Ctrl Pts',(3.81440352439144,-1.5514630336865,12.7063625311661));
#20622=CARTESIAN_POINT('Ctrl Pts',(3.87547414029406,-1.58864064437125,12.7063625311661));
#20623=CARTESIAN_POINT('Ctrl Pts',(3.89458882478181,-1.60027698187568,12.7063625311661));
#20624=CARTESIAN_POINT('Ctrl Pts',(3.91392443695495,-1.61157858690491,12.7063625311661));
#20625=CARTESIAN_POINT('Ctrl Pts',(3.93347817078409,-1.62253437445176,12.7063625311661));
#20626=CARTESIAN_POINT('',(6.25533269723243,1.62367305565468,-5.29454830118707));
#20627=CARTESIAN_POINT('Ctrl Pts',(6.25666079319718,1.62473242747262,-5.29363746883395));
#20628=CARTESIAN_POINT('Ctrl Pts',(6.30029936923465,1.60060502024658,-5.29363746883395));
#20629=CARTESIAN_POINT('Ctrl Pts',(6.34288879700294,1.57478294270003,-5.29363746883395));
#20630=CARTESIAN_POINT('Ctrl Pts',(6.38431760724696,1.54728805898193,-5.29363746883395));
#20631=CARTESIAN_POINT('Ctrl Pts',(6.44434588998498,1.50744934181971,-5.29363746883395));
#20632=CARTESIAN_POINT('Ctrl Pts',(6.50193891059609,1.46410113537834,-5.29363746883395));
#20633=CARTESIAN_POINT('Ctrl Pts',(6.55701390975331,1.4175919904065,-5.29363746883395));
#20634=CARTESIAN_POINT('Ctrl Pts',(6.58791321965453,1.3914984723726,-5.29363746883395));
#20635=CARTESIAN_POINT('Ctrl Pts',(6.61801962391498,1.36440905786912,-5.29363746883395));
#20636=CARTESIAN_POINT('Ctrl Pts',(6.64731552654543,1.33637883922313,-5.29363746883395));
#20637=CARTESIAN_POINT('Ctrl Pts',(6.65793035597894,1.32622260701332,-5.29363746883395));
#20638=CARTESIAN_POINT('Ctrl Pts',(6.66843905008924,1.31594252779162,-5.29363746883395));
#20639=CARTESIAN_POINT('Ctrl Pts',(6.67883979765888,1.30554198152458,-5.29363746883395));
#20640=CARTESIAN_POINT('Ctrl Pts',(6.731109861527,1.2532729293241,-5.29363746883395));
#20641=CARTESIAN_POINT('Ctrl Pts',(6.78048306833212,1.19813763446167,-5.29363746883395));
#20642=CARTESIAN_POINT('Ctrl Pts',(6.82687614202416,1.1405003640249,-5.29363746883395));
#20643=CARTESIAN_POINT('Ctrl Pts',(6.87457429265904,1.0812417077495,-5.29363746883395));
#20644=CARTESIAN_POINT('Ctrl Pts',(6.9191229398719,1.01933778227313,-5.29363746883395));
#20645=CARTESIAN_POINT('Ctrl Pts',(6.96040442051302,0.95513715488343,-5.29363746883395));
#20646=CARTESIAN_POINT('Ctrl Pts',(6.97007751070159,0.940093642653284,-5.29363746883395));
#20647=CARTESIAN_POINT('Ctrl Pts',(6.97957107437076,0.924923849450251,-5.29363746883395));
#20648=CARTESIAN_POINT('Ctrl Pts',(6.98888332827715,0.9096319518153,-5.29363746883395));
#20649=CARTESIAN_POINT('Ctrl Pts',(6.99596956207693,0.89799546048109,-5.29363746883395));
#20650=CARTESIAN_POINT('Ctrl Pts',(7.00295080503329,0.886288261447592,-5.29363746883395));
#20651=CARTESIAN_POINT('Ctrl Pts',(7.00982622720321,0.87451215610694,-5.29363746883395));
#20652=CARTESIAN_POINT('Ctrl Pts',(7.01689812932228,0.862399523274394,-5.29363746883395));
#20653=CARTESIAN_POINT('Ctrl Pts',(7.02385346834336,0.850221843496349,-5.29363746883395));
#20654=CARTESIAN_POINT('Ctrl Pts',(7.03069026763827,0.837984069217663,-5.29363746883395));
#20655=CARTESIAN_POINT('Ctrl Pts',(7.0688520410006,0.769675033316855,-5.29363746883395));
#20656=CARTESIAN_POINT('Ctrl Pts',(7.10333816565241,0.699471189973925,-5.29363746883395));
#20657=CARTESIAN_POINT('Ctrl Pts',(7.1340509191707,0.627756354610849,-5.29363746883395));
#20658=CARTESIAN_POINT('Ctrl Pts',(7.16512437454675,0.555199273881231,-5.29363746883395));
#20659=CARTESIAN_POINT('Ctrl Pts',(7.19233595085917,0.481094685903242,-5.29363746883395));
#20660=CARTESIAN_POINT('Ctrl Pts',(7.21554881768624,0.405800158113758,-5.29363746883395));
#20661=CARTESIAN_POINT('Ctrl Pts',(7.2386023964655,0.331022305771233,-5.29363746883395));
#20662=CARTESIAN_POINT('Ctrl Pts',(7.25771249741322,0.2550698512193,-5.29363746883395));
#20663=CARTESIAN_POINT('Ctrl Pts',(7.27270144705816,0.178267214732533,-5.29363746883395));
#20664=CARTESIAN_POINT('Ctrl Pts',(7.2773482629243,0.154457160109444,-5.29363746883395));
#20665=CARTESIAN_POINT('Ctrl Pts',(7.28159864515951,0.130565261658507,-5.29363746883395));
#20666=CARTESIAN_POINT('Ctrl Pts',(7.28544631241327,0.106600894764324,-5.29363746883395));
#20667=CARTESIAN_POINT('Ctrl Pts',(7.28782821378857,0.0917657349911405,
-5.29363746883395));
#20668=CARTESIAN_POINT('Ctrl Pts',(7.29005592416018,0.0769009007266584,
-5.29363746883395));
#20669=CARTESIAN_POINT('Ctrl Pts',(7.2921251510253,0.0620305370594762,-5.29363746883395));
#20670=CARTESIAN_POINT('Ctrl Pts',(7.30329430528889,-0.0182358602865081,
-5.29363746883395));
#20671=CARTESIAN_POINT('Ctrl Pts',(7.30987324050768,-0.0988001668559794,
-5.29363746883395));
#20672=CARTESIAN_POINT('Ctrl Pts',(7.31173319533953,-0.179285772036483,
-5.29363746883395));
#20673=CARTESIAN_POINT('Ctrl Pts',(7.31242671300975,-0.209296280052594,
-5.29363746883395));
#20674=CARTESIAN_POINT('Ctrl Pts',(7.31246371580651,-0.239296136201682,
-5.29363746883395));
#20675=CARTESIAN_POINT('Ctrl Pts',(7.31183589213809,-0.269266694326119,
-5.29363746883395));
#20676=CARTESIAN_POINT('Ctrl Pts',(7.3101929237976,-0.347697439488371,-5.29363746883395));
#20677=CARTESIAN_POINT('Ctrl Pts',(7.30400105115064,-0.425927024337316,
-5.29363746883395));
#20678=CARTESIAN_POINT('Ctrl Pts',(7.29350020192805,-0.503697173141665,
-5.29363746883395));
#20679=CARTESIAN_POINT('Ctrl Pts',(7.28299935270546,-0.581467321946014,
-5.29363746883395));
#20680=CARTESIAN_POINT('Ctrl Pts',(7.26818923120758,-0.65877879964822,-5.29363746883395));
#20681=CARTESIAN_POINT('Ctrl Pts',(7.24925749796867,-0.735375178179596,
-5.29363746883395));
#20682=CARTESIAN_POINT('Ctrl Pts',(7.24622536278699,-0.747642970631759,
-5.29363746883395));
#20683=CARTESIAN_POINT('Ctrl Pts',(7.24308680695059,-0.759894624142244,
-5.29363746883395));
#20684=CARTESIAN_POINT('Ctrl Pts',(7.2398444115817,-0.772121842590014,-5.29363746883395));
#20685=CARTESIAN_POINT('Ctrl Pts',(7.21915333483621,-0.850148821568037,
-5.29363746883395));
#20686=CARTESIAN_POINT('Ctrl Pts',(7.19429464267757,-0.926973379788445,
-5.29363746883395));
#20687=CARTESIAN_POINT('Ctrl Pts',(7.16554718013261,-1.00232735033283,-5.29363746883395));
#20688=CARTESIAN_POINT('Ctrl Pts',(7.13626789340404,-1.07907535917899,-5.29363746883395));
#20689=CARTESIAN_POINT('Ctrl Pts',(7.10295442700467,-1.15429867121524,-5.29363746883395));
#20690=CARTESIAN_POINT('Ctrl Pts',(7.06584639520479,-1.22771683525656,-5.29363746883395));
#20691=CARTESIAN_POINT('Ctrl Pts',(7.02829731740499,-1.30200760789503,-5.29363746883395));
#20692=CARTESIAN_POINT('Ctrl Pts',(6.98686265169164,-1.37445097862862,-5.29363746883395));
#20693=CARTESIAN_POINT('Ctrl Pts',(6.94173861538553,-1.44474621559212,-5.29363746883395));
#20694=CARTESIAN_POINT('Ctrl Pts',(6.9137828184364,-1.48829638379319,-5.29363746883395));
#20695=CARTESIAN_POINT('Ctrl Pts',(6.88440995680354,-1.53102180418571,-5.29363746883395));
#20696=CARTESIAN_POINT('Ctrl Pts',(6.85365761921674,-1.57284665132636,-5.29363746883395));
#20697=CARTESIAN_POINT('Ctrl Pts',(6.84595894636615,-1.58331726398313,-5.29363746883395));
#20698=CARTESIAN_POINT('Ctrl Pts',(6.83817934135279,-1.59372384382491,-5.29363746883395));
#20699=CARTESIAN_POINT('Ctrl Pts',(6.83032080761261,-1.60406400041825,-5.29363746883395));
#20700=CARTESIAN_POINT('Ctrl Pts',(6.77836195742938,-1.67243078041412,-5.29363746883395));
#20701=CARTESIAN_POINT('Ctrl Pts',(6.72294242113773,-1.73791443631007,-5.29363746883395));
#20702=CARTESIAN_POINT('Ctrl Pts',(6.66431733044397,-1.80021839569566,-5.29363746883395));
#20703=CARTESIAN_POINT('Ctrl Pts',(6.60562811837204,-1.86259050023369,-5.29363746883395));
#20704=CARTESIAN_POINT('Ctrl Pts',(6.54372589764592,-1.92177688286241,-5.29363746883395));
#20705=CARTESIAN_POINT('Ctrl Pts',(6.47881773090058,-1.97746203272859,-5.29363746883395));
#20706=CARTESIAN_POINT('Ctrl Pts',(6.41530242565524,-2.03195223740901,-5.29363746883395));
#20707=CARTESIAN_POINT('Ctrl Pts',(6.348908239579,-2.08309064270886,-5.29363746883395));
#20708=CARTESIAN_POINT('Ctrl Pts',(6.27979002010412,-2.1305519155269,-5.29363746883395));
#20709=CARTESIAN_POINT('Ctrl Pts',(6.24357415776808,-2.1554201910081,-5.29363746883395));
#20710=CARTESIAN_POINT('Ctrl Pts',(6.20660982183934,-2.17927836310074,-5.29363746883395));
#20711=CARTESIAN_POINT('Ctrl Pts',(6.1689156158044,-2.20207516956608,-5.29363746883395));
#20712=CARTESIAN_POINT('Ctrl Pts',(6.25440237736867,1.62237255794581,-5.29454830118707));
#20713=CARTESIAN_POINT('Ctrl Pts',(6.24705183310046,1.62763081968323,-5.29424469040269));
#20714=CARTESIAN_POINT('Ctrl Pts',(6.23966555258041,1.63283912556818,-5.29394107961832));
#20715=CARTESIAN_POINT('Ctrl Pts',(6.2322442180908,1.63799699450132,-5.29363746883395));
#20716=CARTESIAN_POINT('Ctrl Pts',(3.66734314315846,1.99639467351756,-5.55864130264131));
#20717=CARTESIAN_POINT('Ctrl Pts',(3.00418308807966,1.52257887569804,-5.5163482439231));
#20718=CARTESIAN_POINT('Ctrl Pts',(2.19870851602258,-0.129205714733684,
-5.4317794273688));
#20719=CARTESIAN_POINT('Ctrl Pts',(3.63167818438598,-2.50507698344247,-5.30493485297845));
#20720=CARTESIAN_POINT('Ctrl Pts',(6.40036668721888,-2.58655864996601,-5.17810757947023));
#20721=CARTESIAN_POINT('Ctrl Pts',(7.97575989825059,-0.310608158848719,
-5.05128030596201));
#20722=CARTESIAN_POINT('Ctrl Pts',(6.92074750039589,2.25078850093184,-4.92445303245379));
#20723=CARTESIAN_POINT('Ctrl Pts',(4.19787642714988,2.7565776590141,-4.79762575894558));
#20724=CARTESIAN_POINT('Ctrl Pts',(2.29295576704817,0.74658145406325,-4.67079848543737));
#20725=CARTESIAN_POINT('Ctrl Pts',(2.94473032594405,-1.94519874334173,-4.54397121192914));
#20726=CARTESIAN_POINT('Ctrl Pts',(5.55830877699676,-2.86118176505069,-4.41714393842093));
#20727=CARTESIAN_POINT('Ctrl Pts',(7.7478771670619,-1.16544357738298,-4.29031666491272));
#20728=CARTESIAN_POINT('Ctrl Pts',(7.51473324745422,1.59419635928178,-4.16348939140448));
#20729=CARTESIAN_POINT('Ctrl Pts',(5.07168913436726,2.89857139725113,-4.03666211789627));
#20730=CARTESIAN_POINT('Ctrl Pts',(2.64885538638093,1.55702956562814,-3.90983484438807));
#20731=CARTESIAN_POINT('Ctrl Pts',(2.45788523332366,-1.20583472037831,-3.78300757087985));
#20732=CARTESIAN_POINT('Ctrl Pts',(4.67310514312105,-2.86796350212083,-3.65618029737162));
#20733=CARTESIAN_POINT('Ctrl Pts',(7.27237606698426,-1.91210608623046,-3.52935302386342));
#20734=CARTESIAN_POINT('Ctrl Pts',(7.88298359976007,0.789196405494946,-3.4025257503552));
#20735=CARTESIAN_POINT('Ctrl Pts',(5.94754139353568,2.7700895179055,-3.27569847684697));
#20736=CARTESIAN_POINT('Ctrl Pts',(3.23279591815959,2.22233822425849,-3.14887120333877));
#20737=CARTESIAN_POINT('Ctrl Pts',(2.21687156983362,-0.354049302176947,
-3.02204392983055));
#20738=CARTESIAN_POINT('Ctrl Pts',(3.82714334007257,-2.60724689614626,-2.89521665632232));
#20739=CARTESIAN_POINT('Ctrl Pts',(6.59369298446895,-2.4804489182506,-2.76838938281411));
#20740=CARTESIAN_POINT('Ctrl Pts',(7.9911072091958,-0.089401406352042,-2.6415621093059));
#20741=CARTESIAN_POINT('Ctrl Pts',(6.74377236583368,2.3832551509499,-2.51473483579769));
#20742=CARTESIAN_POINT('Ctrl Pts',(3.99030384829488,2.6803844189262,-2.38790756228946));
#20743=CARTESIAN_POINT('Ctrl Pts',(2.2441740004847,0.530755325408102,-2.26108028878124));
#20744=CARTESIAN_POINT('Ctrl Pts',(3.09931754781707,-2.10336771468319,-2.13425301527302));
#20745=CARTESIAN_POINT('Ctrl Pts',(5.77512645185915,-2.81745551666232,-2.00742574176481));
#20746=CARTESIAN_POINT('Ctrl Pts',(7.82901906042506,-0.959661170423007,
-1.88059846825659));
#20747=CARTESIAN_POINT('Ctrl Pts',(7.3861229211855,1.77414893438375,-1.75377119474838));
#20748=CARTESIAN_POINT('Ctrl Pts',(4.85073072563859,2.88844741080586,-1.62694392124016));
#20749=CARTESIAN_POINT('Ctrl Pts',(2.53724633460654,1.36605959809925,-1.50011664773194));
#20750=CARTESIAN_POINT('Ctrl Pts',(2.55750759947128,-1.40332014487893,-1.37328937422373));
#20751=CARTESIAN_POINT('Ctrl Pts',(4.89301925558316,-2.89169509223513,-1.24646210071551));
#20752=CARTESIAN_POINT('Ctrl Pts',(7.4118361137729,-1.74041914154042,-1.11963482720729));
#20753=CARTESIAN_POINT('Ctrl Pts',(7.81468492092802,0.99957858077657,-0.992807553699079));
#20754=CARTESIAN_POINT('Ctrl Pts',(5.73382973613445,2.82712239137559,-0.865980280190864));
#20755=CARTESIAN_POINT('Ctrl Pts',(3.06875549194474,2.0739597577458,-0.739153006682644));
#20756=CARTESIAN_POINT('Ctrl Pts',(2.25224482886564,-0.57239339646756,-0.612325733174432));
#20757=CARTESIAN_POINT('Ctrl Pts',(4.02964019702116,-2.69624376431319,-0.485498459666212));
#20758=CARTESIAN_POINT('Ctrl Pts',(6.77846649786872,-2.35885875055705,-0.358671186157998));
#20759=CARTESIAN_POINT('Ctrl Pts',(7.98948898080085,0.131783581366781,-0.23184391264978));
#20760=CARTESIAN_POINT('Ctrl Pts',(6.55723957859082,2.50212877344481,-0.105016639141564));
#20761=CARTESIAN_POINT('Ctrl Pts',(3.7891308296205,2.58843424031846,0.021810634366653));
#20762=CARTESIAN_POINT('Ctrl Pts',(2.21199924743569,0.311917020481634,0.148637907874869));
#20763=CARTESIAN_POINT('Ctrl Pts',(3.26551141667232,-2.24933009547745,0.275465181383086));
#20764=CARTESIAN_POINT('Ctrl Pts',(5.98798076425687,-2.75730187737167,0.402292454891301));
#20765=CARTESIAN_POINT('Ctrl Pts',(7.89423218388447,-0.748302075254695,
0.529119728399519));
#20766=CARTESIAN_POINT('Ctrl Pts',(7.24416579945549,1.94377674520614,0.655947001907735));
#20767=CARTESIAN_POINT('Ctrl Pts',(4.63118729888403,2.86150112392219,0.782774275415952));
#20768=CARTESIAN_POINT('Ctrl Pts',(2.44052431703461,1.1671368243417,0.909601548924168));
#20769=CARTESIAN_POINT('Ctrl Pts',(2.67189858213383,-1.59263501934178,1.03642882243239));
#20770=CARTESIAN_POINT('Ctrl Pts',(5.11410273407891,-2.89858814252828,1.16325609594061));
#20771=CARTESIAN_POINT('Ctrl Pts',(7.53779855522807,-1.55859812529596,1.29008336944882));
#20772=CARTESIAN_POINT('Ctrl Pts',(7.73054294670161,1.20414042174279,1.41691064295704));
#20773=CARTESIAN_POINT('Ctrl Pts',(5.51639138813421,2.8676931126522,1.54373791646525));
#20774=CARTESIAN_POINT('Ctrl Pts',(2.91650688722692,1.91350483894491,1.67056518997347));
#20775=CARTESIAN_POINT('Ctrl Pts',(2.30416437052955,-0.787404511992841,
1.79739246348169));
#20776=CARTESIAN_POINT('Ctrl Pts',(4.23833372337011,-2.76954063099948,1.92421973698991));
#20777=CARTESIAN_POINT('Ctrl Pts',(6.9534305025952,-2.22353315927424,2.05104701049812));
#20778=CARTESIAN_POINT('Ctrl Pts',(7.97100956687557,0.352201207401914,2.17787428400634));
#20779=CARTESIAN_POINT('Ctrl Pts',(6.36218546834003,2.60643271718737,2.30470155751455));
#20780=CARTESIAN_POINT('Ctrl Pts',(3.59555494386324,2.48141183584503,2.43152883102277));
#20781=CARTESIAN_POINT('Ctrl Pts',(2.19660512661465,0.0912624496018655,
2.55835610453099));
#20782=CARTESIAN_POINT('Ctrl Pts',(3.44235140847758,-2.38219482331856,2.6851833780392));
#20783=CARTESIAN_POINT('Ctrl Pts',(6.19562849824152,-2.68109271009487,2.81201065154742));
#20784=CARTESIAN_POINT('Ctrl Pts',(7.9431387933782,-0.532585682382451,2.93883792505564));
#20785=CARTESIAN_POINT('Ctrl Pts',(7.08968744354401,2.10208611372509,3.06566519856385));
#20786=CARTESIAN_POINT('Ctrl Pts',(4.41433778362352,2.81789256584859,3.19249247207207));
#20787=CARTESIAN_POINT('Ctrl Pts',(2.35925225022766,0.96141791475166,3.31931974558028));
#20788=CARTESIAN_POINT('Ctrl Pts',(2.80039224341925,-1.77267611913694,3.4461470190885));
#20789=CARTESIAN_POINT('Ctrl Pts',(5.3350681496502,-2.88860296714743,3.57297429259672));
#20790=CARTESIAN_POINT('Ctrl Pts',(7.64952996460744,-1.36770152824906,3.69980156610494));
#20791=CARTESIAN_POINT('Ctrl Pts',(7.63104760663617,1.40169065816697,3.82662883961315));
#20792=CARTESIAN_POINT('Ctrl Pts',(5.29649248550149,2.89156550731442,3.95345611312137));
#20793=CARTESIAN_POINT('Ctrl Pts',(2.77693662832761,1.74190774853615,4.08028338662959));
#20794=CARTESIAN_POINT('Ctrl Pts',(2.37232787502268,-0.997830639793556,
4.2071106601378));
#20795=CARTESIAN_POINT('Ctrl Pts',(4.45200871328031,-2.82671070440203,4.33393793364602));
#20796=CARTESIAN_POINT('Ctrl Pts',(7.11756619939457,-2.07526012854318,4.46076520715423));
#20797=CARTESIAN_POINT('Ctrl Pts',(7.93577657097738,0.570567996557279,4.58759248066245));
#20798=CARTESIAN_POINT('Ctrl Pts',(6.15974581837457,2.69555963078725,4.71441975417067));
#20799=CARTESIAN_POINT('Ctrl Pts',(3.41070336637887,2.35994038690525,4.84124702767889));
#20800=CARTESIAN_POINT('Ctrl Pts',(2.19808127670905,-0.129923534553724,
4.9680743011871));
#20801=CARTESIAN_POINT('Ctrl Pts',(3.62880779936598,-2.5011882386946,5.09490157469532));
#20802=CARTESIAN_POINT('Ctrl Pts',(6.39686053920616,-2.58927177405525,5.22172884820352));
#20803=CARTESIAN_POINT('Ctrl Pts',(7.97545410997968,-0.31376808958212,5.34855612171176));
#20804=CARTESIAN_POINT('Ctrl Pts',(6.92358736743495,2.24815521833844,5.47538339521996));
#20805=CARTESIAN_POINT('Ctrl Pts',(4.20144487564846,2.75787566539626,5.60221066872819));
#20806=CARTESIAN_POINT('Ctrl Pts',(2.29390337433622,0.750100752586105,5.72903794223639));
#20807=CARTESIAN_POINT('Ctrl Pts',(2.94224037595603,-1.94239508066396,5.85586521574462));
#20808=CARTESIAN_POINT('Ctrl Pts',(5.55462883997521,-2.86179770889484,5.98269248925282));
#20809=CARTESIAN_POINT('Ctrl Pts',(7.7463797396693,-1.16884092461813,6.10951976276106));
#20810=CARTESIAN_POINT('Ctrl Pts',(7.51677825340999,1.59107897227123,6.23634703626926));
#20811=CARTESIAN_POINT('Ctrl Pts',(5.07541348034676,2.89860056849218,6.36317430977749));
#20812=CARTESIAN_POINT('Ctrl Pts',(2.6508574206784,1.56016768139483,6.4900015832857));
#20813=CARTESIAN_POINT('Ctrl Pts',(2.45633843220973,-1.20244648690003,6.61682885679392));
#20814=CARTESIAN_POINT('Ctrl Pts',(4.66942095594169,-2.86742108817495,6.74365613030213));
#20815=CARTESIAN_POINT('Ctrl Pts',(7.26991784043513,-1.91490303927604,6.87048340381035));
#20816=CARTESIAN_POINT('Ctrl Pts',(7.8839951517652,0.785612418085389,6.99731067731856));
#20817=CARTESIAN_POINT('Ctrl Pts',(5.95109941710099,2.76899053600824,7.12413795082678));
#20818=CARTESIAN_POINT('Ctrl Pts',(3.23565247176357,2.22472721114061,7.250965224335));
#20819=CARTESIAN_POINT('Ctrl Pts',(2.21641910222577,-0.350352985311341,
7.37779249784321));
#20820=CARTESIAN_POINT('Ctrl Pts',(3.823794870053,-2.6056174533372,7.50461977135142));
#20821=CARTESIAN_POINT('Ctrl Pts',(6.59050513054598,-2.4823737345465,7.63144704485966));
#20822=CARTESIAN_POINT('Ctrl Pts',(7.9909899644218,-0.0931234525913811,
7.75827431836786));
#20823=CARTESIAN_POINT('Ctrl Pts',(6.74683275736921,2.38113351140325,7.88510159187608));
#20824=CARTESIAN_POINT('Ctrl Pts',(3.99374823177407,2.68179989573667,8.0119288653843));
#20825=CARTESIAN_POINT('Ctrl Pts',(2.2448582101591,0.534415819229491,8.13875613889251));
#20826=CARTESIAN_POINT('Ctrl Pts',(3.09661701045288,-2.10080364522705,8.26558341240074));
#20827=CARTESIAN_POINT('Ctrl Pts',(5.7715063223249,-2.818328452451,8.39241068590894));
#20828=CARTESIAN_POINT('Ctrl Pts',(7.82778393262807,-0.963174262331539,
8.51923795941717));
#20829=CARTESIAN_POINT('Ctrl Pts',(7.38840026749263,1.77120257243064,8.64606523292537));
#20830=CARTESIAN_POINT('Ctrl Pts',(4.85444169640936,2.88875733165284,8.7728925064336));
#20831=CARTESIAN_POINT('Ctrl Pts',(2.53900341250707,1.3693428940367,8.89971977994182));
#20832=CARTESIAN_POINT('Ctrl Pts',(2.55570685593279,-1.40006059304758,9.02654705345002));
#20833=CARTESIAN_POINT('Ctrl Pts',(4.88930447888277,-2.89143472940734,9.15337432695825));
#20834=CARTESIAN_POINT('Ctrl Pts',(7.40959829534611,-1.74339563661343,9.28020160046646));
#20835=CARTESIAN_POINT('Ctrl Pts',(7.81596682804957,0.996082286734809,9.40702887397467));
#20836=CARTESIAN_POINT('Ctrl Pts',(5.73746119405384,2.82629785178745,9.53385614748291));
#20837=CARTESIAN_POINT('Ctrl Pts',(3.07142156655589,2.07655964175948,9.6606834209911));
#20838=CARTESIAN_POINT('Ctrl Pts',(2.25151182272583,-0.568742358732331,
9.78751069449933));
#20839=CARTESIAN_POINT('Ctrl Pts',(4.02617722953086,-2.69487438979598,9.91433796800753));
#20840=CARTESIAN_POINT('Ctrl Pts',(6.77543469351166,-2.36102104047297,10.0411652415158));
#20841=CARTESIAN_POINT('Ctrl Pts',(7.98965589887894,0.128063416899711,10.1679925150239));
#20842=CARTESIAN_POINT('Ctrl Pts',(6.56045282839116,2.50024670475965,10.2948197885321));
#20843=CARTESIAN_POINT('Ctrl Pts',(3.79245727355498,2.59010817689208,10.4216470620404));
#20844=CARTESIAN_POINT('Ctrl Pts',(2.21240230124421,0.315619148361449,10.5484743355487));
#20845=CARTESIAN_POINT('Ctrl Pts',(3.26262330556337,-2.24697964055797,10.6753016090568));
#20846=CARTESIAN_POINT('Ctrl Pts',(5.98443758504871,-2.75844788311353,10.802128882565));
#20847=CARTESIAN_POINT('Ctrl Pts',(7.8932688254564,-0.751899944113938,10.9289561560733));
#20848=CARTESIAN_POINT('Ctrl Pts',(7.24666062741032,1.94101418382779,11.0557834295814));
#20849=CARTESIAN_POINT('Ctrl Pts',(4.63486489090856,2.86209012378437,11.1826107030897));
#20850=CARTESIAN_POINT('Ctrl Pts',(2.4420239047778,1.17055023725741,11.3094379765979));
#20851=CARTESIAN_POINT('Ctrl Pts',(2.66985837145817,-1.58953311711393,11.4362652501061));
#20852=CARTESIAN_POINT('Ctrl Pts',(5.11037160631846,-2.89859113200809,11.5630925236143));
#20853=CARTESIAN_POINT('Ctrl Pts',(7.53580814890384,-1.56177596387239,11.6899197971225));
#20854=CARTESIAN_POINT('Ctrl Pts',(7.73206118220609,1.20082705749807,11.8167470706307));
#20855=CARTESIAN_POINT('Ctrl Pts',(5.52012570729668,2.86700499518553,11.9435743441391));
#20856=CARTESIAN_POINT('Ctrl Pts',(2.9188706246569,1.91657269933589,12.0704016176473));
#20857=CARTESIAN_POINT('Ctrl Pts',(2.30333867231827,-0.784339077085607,
12.1972288911554));
#20858=CARTESIAN_POINT('Ctrl Pts',(4.23442611238473,-2.76744666524104,12.3240561646636));
#20859=CARTESIAN_POINT('Ctrl Pts',(6.95124491673232,-2.22784415223559,12.4508834381719));
#20860=CARTESIAN_POINT('Ctrl Pts',(7.97013296042037,0.352453055628561,12.57771071168));
#20861=CARTESIAN_POINT('Ctrl Pts',(6.9024066677663,1.84748978079073,12.6622622273523));
#20862=CARTESIAN_POINT('Ctrl Pts',(6.17030206810482,2.20491500302837,12.7045379851883));
#20863=CARTESIAN_POINT('Ctrl Pts',(3.75695945986218,1.87097473485327,-5.46964458820123));
#20864=CARTESIAN_POINT('Ctrl Pts',(3.13546125378344,1.42692557039988,-5.42735152948301));
#20865=CARTESIAN_POINT('Ctrl Pts',(2.38058918671353,-0.121088595893445,
-5.34278271292872));
#20866=CARTESIAN_POINT('Ctrl Pts',(3.72353508858527,-2.34769998490586,-5.21593813853836));
#20867=CARTESIAN_POINT('Ctrl Pts',(6.31828566881595,-2.42406271089463,-5.08911086503014));
#20868=CARTESIAN_POINT('Ctrl Pts',(7.79470760802413,-0.29109475463651,-4.96228359152192));
#20869=CARTESIAN_POINT('Ctrl Pts',(6.80597448449539,2.10938672327844,-4.83545631801371));
#20870=CARTESIAN_POINT('Ctrl Pts',(4.25416293546439,2.58340057859856,-4.70862904450549));
#20871=CARTESIAN_POINT('Ctrl Pts',(2.46891552210067,0.699678804292331,-4.58180177099727));
#20872=CARTESIAN_POINT('Ctrl Pts',(3.07974350551026,-1.82299509778206,-4.45497449748906));
#20873=CARTESIAN_POINT('Ctrl Pts',(5.52912854662575,-2.68143311803203,-4.32814722398084));
#20874=CARTESIAN_POINT('Ctrl Pts',(7.58114120343533,-1.09222666094304,-4.20131995047263));
#20875=CARTESIAN_POINT('Ctrl Pts',(7.36264413521682,1.49404381316841,-4.0744926769644));
#20876=CARTESIAN_POINT('Ctrl Pts',(5.07307991610174,2.7164738132014,-3.94766540345619));
#20877=CARTESIAN_POINT('Ctrl Pts',(2.80245638190584,1.45921195711113,-3.82083812994798));
#20878=CARTESIAN_POINT('Ctrl Pts',(2.62348358848939,-1.13008030233899,-3.69401085643976));
#20879=CARTESIAN_POINT('Ctrl Pts',(4.69953625400377,-2.68778880455282,-3.56718358293154));
#20880=CARTESIAN_POINT('Ctrl Pts',(7.13551261283571,-1.79198142789719,-3.44035630942333));
#20881=CARTESIAN_POINT('Ctrl Pts',(7.7077598151996,0.739616547321491,-3.31352903591511));
#20882=CARTESIAN_POINT('Ctrl Pts',(5.89390831747238,2.59606357902733,-3.1867017624069));
#20883=CARTESIAN_POINT('Ctrl Pts',(3.34971189010135,2.08272378455118,-3.05987448889867));
#20884=CARTESIAN_POINT('Ctrl Pts',(2.3976111790275,-0.331806785528213,-2.93304721539046));
#20885=CARTESIAN_POINT('Ctrl Pts',(3.906720494099,-2.443451254866,-2.80621994188224));
#20886=CARTESIAN_POINT('Ctrl Pts',(6.49946658586394,-2.32461913403326,-2.67939266837402));
#20887=CARTESIAN_POINT('Ctrl Pts',(7.80909075150137,-0.0837849222720541,
-2.55256539486581));
#20888=CARTESIAN_POINT('Ctrl Pts',(6.64011749747002,2.23353139200658,-2.42573812135759));
#20889=CARTESIAN_POINT('Ctrl Pts',(4.05963073407268,2.51199404307626,-2.29891084784938));
#20890=CARTESIAN_POINT('Ctrl Pts',(2.42319838311386,0.497411567662471,-2.17208357434116));
#20891=CARTESIAN_POINT('Ctrl Pts',(3.22461906057571,-1.97122738528671,-2.04525630083294));
#20892=CARTESIAN_POINT('Ctrl Pts',(5.7323250373389,-2.64045389329767,-1.91842902732473));
#20893=CARTESIAN_POINT('Ctrl Pts',(7.65718550190721,-0.899372167086362,
-1.79160175381651));
#20894=CARTESIAN_POINT('Ctrl Pts',(7.24211352356873,1.66269118833614,-1.66477448030829));
#20895=CARTESIAN_POINT('Ctrl Pts',(4.86600282575051,2.70698584816805,-1.53794720680008));
#20896=CARTESIAN_POINT('Ctrl Pts',(2.6978589699708,1.28023933756755,-1.41111993329186));
#20897=CARTESIAN_POINT('Ctrl Pts',(2.71684735696714,-1.31515905687775,-1.28429265978365));
#20898=CARTESIAN_POINT('Ctrl Pts',(4.90563465414091,-2.71002949979746,-1.15746538627543));
#20899=CARTESIAN_POINT('Ctrl Pts',(7.26621133064149,-1.63108040963648,-1.03063811276721));
#20900=CARTESIAN_POINT('Ctrl Pts',(7.64375187918689,0.936781837249784,-0.903810839258996));
#20901=CARTESIAN_POINT('Ctrl Pts',(5.69362271420696,2.64951346382921,-0.776983565750779));
#20902=CARTESIAN_POINT('Ctrl Pts',(3.19597701141537,1.94366693085183,-0.650156292242562));
#20903=CARTESIAN_POINT('Ctrl Pts',(2.43076217608045,-0.536433801088405,
-0.523329018734348));
#20904=CARTESIAN_POINT('Ctrl Pts',(4.09649584677037,-2.52685705334372,-0.39650174522613));
#20905=CARTESIAN_POINT('Ctrl Pts',(6.67263203246968,-2.21066765200472,-0.269674471717914));
#20906=CARTESIAN_POINT('Ctrl Pts',(7.80757418542239,0.123504512647947,-0.142847198209698));
#20907=CARTESIAN_POINT('Ctrl Pts',(6.4653033002661,2.34493699094889,-0.0160199247014798));
#20908=CARTESIAN_POINT('Ctrl Pts',(3.87109605189446,2.42582047062467,0.110807348806736));
#20909=CARTESIAN_POINT('Ctrl Pts',(2.39304495160387,0.292321389369155,0.237634622314952));
#20910=CARTESIAN_POINT('Ctrl Pts',(3.3803720957047,-2.10801993954849,0.364461895823169));
#20911=CARTESIAN_POINT('Ctrl Pts',(5.93180715677322,-2.58407929922806,0.491289169331385));
#20912=CARTESIAN_POINT('Ctrl Pts',(7.71830172706644,-0.701291330522815,
0.618116442839602));
#20913=CARTESIAN_POINT('Ctrl Pts',(7.10907460510611,1.82166243414596,0.744943716347819));
#20914=CARTESIAN_POINT('Ctrl Pts',(4.66025182365174,2.68173241375138,0.871770989856034));
#20915=CARTESIAN_POINT('Ctrl Pts',(2.60721334083663,1.09381353267821,0.998598263364254));
#20916=CARTESIAN_POINT('Ctrl Pts',(2.82405192993845,-1.49258056162853,1.12542553687247));
#20917=CARTESIAN_POINT('Ctrl Pts',(5.11282895697391,-2.71648950648634,1.25225281038069));
#20918=CARTESIAN_POINT('Ctrl Pts',(7.38426040612206,-1.46068197481231,1.3790800838889));
#20919=CARTESIAN_POINT('Ctrl Pts',(7.56489597458717,1.12849244499676,1.50590735739712));
#20920=CARTESIAN_POINT('Ctrl Pts',(5.4898445430401,2.68753540182084,1.63273463090533));
#20921=CARTESIAN_POINT('Ctrl Pts',(3.05329315404872,1.79329230646433,1.75956190441355));
#20922=CARTESIAN_POINT('Ctrl Pts',(2.47941996503718,-0.737937226336289,
1.88638917792177));
#20923=CARTESIAN_POINT('Ctrl Pts',(4.29207857412674,-2.59554917496329,2.01321645142998));
#20924=CARTESIAN_POINT('Ctrl Pts',(6.83660423530834,-2.08384364990342,2.1400437249382));
#20925=CARTESIAN_POINT('Ctrl Pts',(7.79025570775473,0.330074794014927,2.26687099844642));
#20926=CARTESIAN_POINT('Ctrl Pts',(6.28250311699098,2.4426882252497,2.39369827195463));
#20927=CARTESIAN_POINT('Ctrl Pts',(3.6896812262926,2.32552155804531,2.52052554546285));
#20928=CARTESIAN_POINT('Ctrl Pts',(2.37861793899785,0.0855290487952711,
2.64735281897107));
#20929=CARTESIAN_POINT('Ctrl Pts',(3.54610243007606,-2.23253767756964,2.77418009247928));
#20930=CARTESIAN_POINT('Ctrl Pts',(6.12640979180747,-2.51265783711412,2.9010073659875));
#20931=CARTESIAN_POINT('Ctrl Pts',(7.76413586594884,-0.499126935720797,
3.02783463949572));
#20932=CARTESIAN_POINT('Ctrl Pts',(6.96430107669211,1.97002629862555,3.15466191300393));
#20933=CARTESIAN_POINT('Ctrl Pts',(4.45702549285675,2.64086348564745,3.28148918651215));
#20934=CARTESIAN_POINT('Ctrl Pts',(2.53104704683569,0.901018547082313,3.40831646002037));
#20935=CARTESIAN_POINT('Ctrl Pts',(2.94447320587293,-1.66131090008331,3.53514373352858));
#20936=CARTESIAN_POINT('Ctrl Pts',(5.3199126139754,-2.7071316319596,3.6619710070368));
#20937=CARTESIAN_POINT('Ctrl Pts',(7.48897248876349,-1.2817781163809,3.78879828054501));
#20938=CARTESIAN_POINT('Ctrl Pts',(7.47165125200432,1.31363193976544,3.91562555405324));
#20939=CARTESIAN_POINT('Ctrl Pts',(5.28376039720189,2.70990805581855,4.04245282756144));
#20940=CARTESIAN_POINT('Ctrl Pts',(2.92249114801181,1.63247549754976,4.16928010106968));
#20941=CARTESIAN_POINT('Ctrl Pts',(2.54330121879797,-0.935143707544964,
4.29610737457787));
#20942=CARTESIAN_POINT('Ctrl Pts',(4.49232981347094,-2.64912764035633,4.4229346480861));
#20943=CARTESIAN_POINT('Ctrl Pts',(6.99042839937408,-1.94488560817054,4.54976192159431));
#20944=CARTESIAN_POINT('Ctrl Pts',(7.75723616205411,0.534723078675424,4.67658919510254));
#20945=CARTESIAN_POINT('Ctrl Pts',(6.09278137737594,2.52621589928772,4.80341646861074));
#20946=CARTESIAN_POINT('Ctrl Pts',(3.51644261983928,2.21168133647635,4.93024374211896));
#20947=CARTESIAN_POINT('Ctrl Pts',(2.38000135259241,-0.121761319962131,
5.05707101562718));
#20948=CARTESIAN_POINT('Ctrl Pts',(3.7208450303904,-2.34405554361875,5.1838982891354));
#20949=CARTESIAN_POINT('Ctrl Pts',(6.3149997883057,-2.42660538779657,5.31072556264361));
#20950=CARTESIAN_POINT('Ctrl Pts',(7.79442103035657,-0.294056168351199,
5.43755283615183));
#20951=CARTESIAN_POINT('Ctrl Pts',(6.80863594194712,2.10691887197262,5.56438010966004));
#20952=CARTESIAN_POINT('Ctrl Pts',(4.25750720254346,2.58461704004224,5.69120738316827));
#20953=CARTESIAN_POINT('Ctrl Pts',(2.46980359764909,0.702977009155337,5.81803465667647));
#20954=CARTESIAN_POINT('Ctrl Pts',(3.07740998219424,-1.82036757021712,5.9448619301847));
#20955=CARTESIAN_POINT('Ctrl Pts',(5.52567979509156,-2.68201036630151,6.07168920369291));
#20956=CARTESIAN_POINT('Ctrl Pts',(7.5797378492509,-1.09541057589074,6.19851647720112));
#20957=CARTESIAN_POINT('Ctrl Pts',(7.36456066731672,1.49112227044299,6.32534375070935));
#20958=CARTESIAN_POINT('Ctrl Pts',(5.07657028668021,2.71650115181121,6.45217102421755));
#20959=CARTESIAN_POINT('Ctrl Pts',(2.80433264196533,1.46215292634553,6.57899829772579));
#20960=CARTESIAN_POINT('Ctrl Pts',(2.62203396239971,-1.12690492859264,6.70582557123398));
#20961=CARTESIAN_POINT('Ctrl Pts',(4.69608351932035,-2.68728046679675,6.83265284474222));
#20962=CARTESIAN_POINT('Ctrl Pts',(7.13320881999005,-1.79460266735062,6.95948011825042));
#20963=CARTESIAN_POINT('Ctrl Pts',(7.70870781825216,0.736257717535846,7.08630739175865));
#20964=CARTESIAN_POINT('Ctrl Pts',(5.89724281454603,2.59503363870986,7.21313466526686));
#20965=CARTESIAN_POINT('Ctrl Pts',(3.35238898581429,2.08496268758856,7.33996193877508));
#20966=CARTESIAN_POINT('Ctrl Pts',(2.39718713689099,-0.328342683184473,
7.4667892122833));
#20967=CARTESIAN_POINT('Ctrl Pts',(3.90358238574292,-2.44192417889846,7.59361648579151));
#20968=CARTESIAN_POINT('Ctrl Pts',(6.4964790031843,-2.32642302717454,7.72044375929973));
#20969=CARTESIAN_POINT('Ctrl Pts',(7.80898087242143,-0.0872731375874623,
7.84727103280795));
#20970=CARTESIAN_POINT('Ctrl Pts',(6.6429856253596,2.23154304068462,7.97409830631615));
#20971=CARTESIAN_POINT('Ctrl Pts',(4.06285873029619,2.51332059507786,8.10092557982439));
#20972=CARTESIAN_POINT('Ctrl Pts',(2.42383960853443,0.500842097480926,8.22775285333259));
#20973=CARTESIAN_POINT('Ctrl Pts',(3.22208817966025,-1.9688243989261,8.35458012684081));
#20974=CARTESIAN_POINT('Ctrl Pts',(5.72893233599315,-2.64127198845061,8.48140740034902));
#20975=CARTESIAN_POINT('Ctrl Pts',(7.65602796881361,-0.902664555254527,
8.60823467385724));
#20976=CARTESIAN_POINT('Ctrl Pts',(7.24424779965137,1.65992992632361,8.73506194736546));
#20977=CARTESIAN_POINT('Ctrl Pts',(4.86948066139391,2.70727629878997,8.86188922087367));
#20978=CARTESIAN_POINT('Ctrl Pts',(2.69950566258259,1.28331636628713,8.9887164943819));
#20979=CARTESIAN_POINT('Ctrl Pts',(2.71515974193331,-1.31210428058311,9.11554376789009));
#20980=CARTESIAN_POINT('Ctrl Pts',(4.90215325166861,-2.70978549380048,9.24237104139833));
#20981=CARTESIAN_POINT('Ctrl Pts',(7.26411409917053,-1.63386991170937,9.36919831490655));
#20982=CARTESIAN_POINT('Ctrl Pts',(7.64495325277734,0.933505191652339,9.49602558841475));
#20983=CARTESIAN_POINT('Ctrl Pts',(5.69702603225222,2.64874072447172,9.62285286192299));
#20984=CARTESIAN_POINT('Ctrl Pts',(3.19847559463885,1.9461034817842,9.74968013543118));
#20985=CARTESIAN_POINT('Ctrl Pts',(2.43007521974548,-0.533012133294348,
9.87650740893942));
#20986=CARTESIAN_POINT('Ctrl Pts',(4.09325043404316,-2.52557370734091,10.0033346824476));
#20987=CARTESIAN_POINT('Ctrl Pts',(6.66979069582002,-2.21269409990892,10.1301619559558));
#20988=CARTESIAN_POINT('Ctrl Pts',(7.80773061716958,0.12001806088582,10.256989229464));
#20989=CARTESIAN_POINT('Ctrl Pts',(6.46831468337235,2.34317315987586,10.3838165029722));
#20990=CARTESIAN_POINT('Ctrl Pts',(3.87421351791502,2.42738924511528,10.5106437764805));
#20991=CARTESIAN_POINT('Ctrl Pts',(2.39342268427494,0.295790937660488,10.6374710499887));
#20992=CARTESIAN_POINT('Ctrl Pts',(3.37766542503081,-2.10581714777185,10.7642983234969));
#20993=CARTESIAN_POINT('Ctrl Pts',(5.92848657148644,-2.58515330920086,10.8911255970051));
#20994=CARTESIAN_POINT('Ctrl Pts',(7.71739888991534,-0.704663169680801,
11.0179528705133));
#20995=CARTESIAN_POINT('Ctrl Pts',(7.11141269993937,1.81907342576453,11.1447801440215));
#20996=CARTESIAN_POINT('Ctrl Pts',(4.66369837750916,2.68228441074656,11.2716074175298));
#20997=CARTESIAN_POINT('Ctrl Pts',(2.60861871965148,1.09701250400869,11.398434691038));
#20998=CARTESIAN_POINT('Ctrl Pts',(2.82213989186371,-1.48967353088191,11.5252619645462));
#20999=CARTESIAN_POINT('Ctrl Pts',(5.10933223066781,-2.71649230815741,11.6520892380544));
#21000=CARTESIAN_POINT('Ctrl Pts',(7.38239504352909,-1.46366017134169,11.7789165115626));
#21001=CARTESIAN_POINT('Ctrl Pts',(7.56631882965092,1.12538723695775,11.9057437850708));
#21002=CARTESIAN_POINT('Ctrl Pts',(5.49334426025409,2.68689051410809,12.0325710585791));
#21003=CARTESIAN_POINT('Ctrl Pts',(3.05550839388582,1.79616743399183,12.1593983320873));
#21004=CARTESIAN_POINT('Ctrl Pts',(2.47864613984498,-0.735064371915841,
12.2862256055955));
#21005=CARTESIAN_POINT('Ctrl Pts',(4.28841645183988,-2.5935867588731,12.4130528791037));
#21006=CARTESIAN_POINT('Ctrl Pts',(6.83455595498352,-2.08788381241227,12.5398801526119));
#21007=CARTESIAN_POINT('Ctrl Pts',(7.78943417253837,0.330310820325419,12.6667074261201));
#21008=CARTESIAN_POINT('Ctrl Pts',(6.78878588200046,1.73142452672881,12.7512589417923));
#21009=CARTESIAN_POINT('Ctrl Pts',(6.10267444952349,2.0663951461543,12.7935346996283));
#21010=CARTESIAN_POINT('Ctrl Pts',(3.8465757765659,1.74555479618898,-5.38064787376115));
#21011=CARTESIAN_POINT('Ctrl Pts',(3.2667394194872,1.33127226510172,-5.33835481504293));
#21012=CARTESIAN_POINT('Ctrl Pts',(2.56246985740446,-0.112971477053206,
-5.25378599848864));
#21013=CARTESIAN_POINT('Ctrl Pts',(3.81539199278459,-2.19032298636925,-5.12694142409827));
#21014=CARTESIAN_POINT('Ctrl Pts',(6.236204650413,-2.26156677182326,-5.00011415059006));
#21015=CARTESIAN_POINT('Ctrl Pts',(7.61365531779766,-0.271581350424303,
-4.87328687708184));
#21016=CARTESIAN_POINT('Ctrl Pts',(6.69120146859492,1.96798494562505,-4.74645960357363));
#21017=CARTESIAN_POINT('Ctrl Pts',(4.31044944377891,2.41022349818302,-4.61963233006541));
#21018=CARTESIAN_POINT('Ctrl Pts',(2.6448752771532,0.652776154521415,-4.4928050565572));
#21019=CARTESIAN_POINT('Ctrl Pts',(3.21475668507646,-1.70079145222239,-4.36597778304898));
#21020=CARTESIAN_POINT('Ctrl Pts',(5.49994831625476,-2.50168447101337,-4.23915050954076));
#21021=CARTESIAN_POINT('Ctrl Pts',(7.41440523980874,-1.01900974450311,-4.11232323603255));
#21022=CARTESIAN_POINT('Ctrl Pts',(7.21055502297941,1.39389126705505,-3.98549596252432));
#21023=CARTESIAN_POINT('Ctrl Pts',(5.07447069783619,2.53437622915167,-3.85866868901612));
#21024=CARTESIAN_POINT('Ctrl Pts',(2.95605737743077,1.36139434859413,-3.73184141550789));
#21025=CARTESIAN_POINT('Ctrl Pts',(2.78908194365509,-1.05432588429969,-3.60501414199968));
#21026=CARTESIAN_POINT('Ctrl Pts',(4.7259673648865,-2.50761410698481,-3.47818686849146));
#21027=CARTESIAN_POINT('Ctrl Pts',(6.99864915868715,-1.67185676956393,-3.35135959498325));
#21028=CARTESIAN_POINT('Ctrl Pts',(7.53253603063915,0.690036689148038,-3.22453232147503));
#21029=CARTESIAN_POINT('Ctrl Pts',(5.84027524140905,2.42203764014914,-3.09770504796681));
#21030=CARTESIAN_POINT('Ctrl Pts',(3.46662786204312,1.94310934484386,-2.9708777744586));
#21031=CARTESIAN_POINT('Ctrl Pts',(2.57835078822135,-0.309564268879482,
-2.84405050095038));
#21032=CARTESIAN_POINT('Ctrl Pts',(3.98629764812545,-2.27965561358574,-2.71722322744216));
#21033=CARTESIAN_POINT('Ctrl Pts',(6.40524018725889,-2.16878934981591,-2.59039595393395));
#21034=CARTESIAN_POINT('Ctrl Pts',(7.62707429380696,-0.0781684381920649,
-2.46356868042573));
#21035=CARTESIAN_POINT('Ctrl Pts',(6.53646262910636,2.08380763306326,-2.33674140691751));
#21036=CARTESIAN_POINT('Ctrl Pts',(4.1289576198505,2.34360366722632,-2.2099141334093));
#21037=CARTESIAN_POINT('Ctrl Pts',(2.60222276574302,0.464067809916839,-2.08308685990108));
#21038=CARTESIAN_POINT('Ctrl Pts',(3.34992057333436,-1.83908705589022,-1.95625958639286));
#21039=CARTESIAN_POINT('Ctrl Pts',(5.68952362281864,-2.46345226993301,-1.82943231288465));
#21040=CARTESIAN_POINT('Ctrl Pts',(7.48535194338934,-0.839083163749716,
-1.70260503937643));
#21041=CARTESIAN_POINT('Ctrl Pts',(7.09810412595198,1.55123344228854,-1.57577776586821));
#21042=CARTESIAN_POINT('Ctrl Pts',(4.88127492586239,2.52552428553024,-1.44895049236));
#21043=CARTESIAN_POINT('Ctrl Pts',(2.85847160533509,1.19441907703585,-1.32212321885178));
#21044=CARTESIAN_POINT('Ctrl Pts',(2.87618711446296,-1.22699796887657,-1.19529594534357));
#21045=CARTESIAN_POINT('Ctrl Pts',(4.91825005269867,-2.52836390735981,-1.06846867183535));
#21046=CARTESIAN_POINT('Ctrl Pts',(7.12058654751004,-1.52174167773256,-0.94164139832713));
#21047=CARTESIAN_POINT('Ctrl Pts',(7.47281883744579,0.873985093723001,-0.814814124818913));
#21048=CARTESIAN_POINT('Ctrl Pts',(5.65341569227946,2.47190453628283,-0.687986851310695));
#21049=CARTESIAN_POINT('Ctrl Pts',(3.32319853088602,1.81337410395784,-0.561159577802478));
#21050=CARTESIAN_POINT('Ctrl Pts',(2.60927952329525,-0.500474205709249,
-0.434332304294264));
#21051=CARTESIAN_POINT('Ctrl Pts',(4.16335149651959,-2.35747034237424,-0.307505030786045));
#21052=CARTESIAN_POINT('Ctrl Pts',(6.56679756707065,-2.06247655345239,-0.18067775727783));
#21053=CARTESIAN_POINT('Ctrl Pts',(7.62565939004391,0.115225443929111,-0.0538504837696133));
#21054=CARTESIAN_POINT('Ctrl Pts',(6.37336702194138,2.18774520845296,0.0729767897386032));
#21055=CARTESIAN_POINT('Ctrl Pts',(3.95306127416843,2.26320670093089,0.199804063246821));
#21056=CARTESIAN_POINT('Ctrl Pts',(2.57409065577204,0.272725758256677,0.326631336755036));
#21057=CARTESIAN_POINT('Ctrl Pts',(3.49523277473707,-1.96670978361953,0.453458610263254));
#21058=CARTESIAN_POINT('Ctrl Pts',(5.8756335492896,-2.41085672108445,0.580285883771469));
#21059=CARTESIAN_POINT('Ctrl Pts',(7.54237127024841,-0.65428058579094,0.707113157279686));
#21060=CARTESIAN_POINT('Ctrl Pts',(6.97398341075674,1.69954812308578,0.833940430787902));
#21061=CARTESIAN_POINT('Ctrl Pts',(4.68931634841942,2.50196370358057,0.960767704296119));
#21062=CARTESIAN_POINT('Ctrl Pts',(2.77390236463867,1.02049024101471,1.08759497780433));
#21063=CARTESIAN_POINT('Ctrl Pts',(2.97620527774305,-1.39252610391526,1.21442225131255));
#21064=CARTESIAN_POINT('Ctrl Pts',(5.11155517986895,-2.53439087044442,1.34124952482077));
#21065=CARTESIAN_POINT('Ctrl Pts',(7.23072225701601,-1.36276582432866,1.46807679832898));
#21066=CARTESIAN_POINT('Ctrl Pts',(7.39924900247276,1.05284446825073,1.5949040718372));
#21067=CARTESIAN_POINT('Ctrl Pts',(5.46329769794598,2.50737769098948,1.72173134534542));
#21068=CARTESIAN_POINT('Ctrl Pts',(3.19007942087056,1.67307977398374,1.84855861885363));
#21069=CARTESIAN_POINT('Ctrl Pts',(2.65467555954479,-0.688469940679736,
1.97538589236185));
#21070=CARTESIAN_POINT('Ctrl Pts',(4.34582342488339,-2.42155771892711,2.10221316587007));
#21071=CARTESIAN_POINT('Ctrl Pts',(6.71977796802145,-1.94415414053259,2.22904043937828));
#21072=CARTESIAN_POINT('Ctrl Pts',(7.6095018486339,0.307948380627944,2.3558677128865));
#21073=CARTESIAN_POINT('Ctrl Pts',(6.20282076564191,2.27894373331201,2.48269498639471));
#21074=CARTESIAN_POINT('Ctrl Pts',(3.78380750872197,2.16963128024559,2.60952225990293));
#21075=CARTESIAN_POINT('Ctrl Pts',(2.56063075138103,0.0797956479886741,
2.73634953341115));
#21076=CARTESIAN_POINT('Ctrl Pts',(3.64985345167457,-2.08288053182072,2.86317680691936));
#21077=CARTESIAN_POINT('Ctrl Pts',(6.05719108537339,-2.34422296413337,2.99000408042758));
#21078=CARTESIAN_POINT('Ctrl Pts',(7.5851329385195,-0.465668189059147,3.11683135393579));
#21079=CARTESIAN_POINT('Ctrl Pts',(6.8389147098402,1.837966483526,3.24365862744402));
#21080=CARTESIAN_POINT('Ctrl Pts',(4.49971320208998,2.4638344054463,3.37048590095223));
#21081=CARTESIAN_POINT('Ctrl Pts',(2.70284184344369,0.840619179412967,3.49731317446045));
#21082=CARTESIAN_POINT('Ctrl Pts',(3.08855416832663,-1.54994568102967,3.62414044796866));
#21083=CARTESIAN_POINT('Ctrl Pts',(5.30475707830057,-2.52566029677176,3.75096772147688));
#21084=CARTESIAN_POINT('Ctrl Pts',(7.32841501291955,-1.19585470451273,3.87779499498509));
#21085=CARTESIAN_POINT('Ctrl Pts',(7.31225489737246,1.22557322136391,4.00462226849332));
#21086=CARTESIAN_POINT('Ctrl Pts',(5.2710283089023,2.52825060432267,4.13144954200153));
#21087=CARTESIAN_POINT('Ctrl Pts',(3.06804566769601,1.52304324656336,4.25827681550975));
#21088=CARTESIAN_POINT('Ctrl Pts',(2.71427456257327,-0.872456775296374,
4.38510408901796));
#21089=CARTESIAN_POINT('Ctrl Pts',(4.53265091366157,-2.47154457631062,4.51193136252618));
#21090=CARTESIAN_POINT('Ctrl Pts',(6.86329059935359,-1.81451108779791,4.63875863603439));
#21091=CARTESIAN_POINT('Ctrl Pts',(7.57869575313083,0.498878160793571,4.76558590954261));
#21092=CARTESIAN_POINT('Ctrl Pts',(6.02581693637731,2.35687216778819,4.89241318305083));
#21093=CARTESIAN_POINT('Ctrl Pts',(3.62218187329969,2.06342228604745,5.01924045655905));
#21094=CARTESIAN_POINT('Ctrl Pts',(2.56192142847576,-0.113599105370537,
5.14606773006726));
#21095=CARTESIAN_POINT('Ctrl Pts',(3.81288226141482,-2.18692284854289,5.27289500357548));
#21096=CARTESIAN_POINT('Ctrl Pts',(6.23313903740525,-2.26393900153788,5.3997222770837));
#21097=CARTESIAN_POINT('Ctrl Pts',(7.61338795073345,-0.274344247120272,
5.52654955059191));
#21098=CARTESIAN_POINT('Ctrl Pts',(6.69368451645931,1.9656825256068,5.65337682410013));
#21099=CARTESIAN_POINT('Ctrl Pts',(4.31356952943847,2.41135841468822,5.78020409760834));
#21100=CARTESIAN_POINT('Ctrl Pts',(2.64570382096195,0.655853265724565,5.90703137111657));
#21101=CARTESIAN_POINT('Ctrl Pts',(3.21257958843244,-1.69834005977028,6.03385864462477));
#21102=CARTESIAN_POINT('Ctrl Pts',(5.49673075020791,-2.50222302370819,6.160685918133));
#21103=CARTESIAN_POINT('Ctrl Pts',(7.4130959588325,-1.02198022716333,6.2875131916412));
#21104=CARTESIAN_POINT('Ctrl Pts',(7.21234308122342,1.39116556861474,6.41434046514944));
#21105=CARTESIAN_POINT('Ctrl Pts',(5.07772709301368,2.53440173513023,6.54116773865764));
#21106=CARTESIAN_POINT('Ctrl Pts',(2.95780786325225,1.36413817129623,6.66799501216586));
#21107=CARTESIAN_POINT('Ctrl Pts',(2.78772949258969,-1.05136337028526,6.79482228567407));
#21108=CARTESIAN_POINT('Ctrl Pts',(4.72274608269899,-2.50713984541855,6.9216495591823));
#21109=CARTESIAN_POINT('Ctrl Pts',(6.99649979954498,-1.67430229542522,7.04847683269051));
#21110=CARTESIAN_POINT('Ctrl Pts',(7.53342048473911,0.686903016986302,7.17530410619872));
#21111=CARTESIAN_POINT('Ctrl Pts',(5.84338621199107,2.42107674141147,7.30213137970695));
#21112=CARTESIAN_POINT('Ctrl Pts',(3.469125499865,1.94519816403651,7.42895865321516));
#21113=CARTESIAN_POINT('Ctrl Pts',(2.57795517155622,-0.306332381057607,
7.55578592672338));
#21114=CARTESIAN_POINT('Ctrl Pts',(3.98336990143284,-2.27823090445972,7.68261320023158));
#21115=CARTESIAN_POINT('Ctrl Pts',(6.40245287582263,-2.17047231980259,7.80944047373982));
#21116=CARTESIAN_POINT('Ctrl Pts',(7.62697178042107,-0.0814228225835379,
7.93626774724802));
#21117=CARTESIAN_POINT('Ctrl Pts',(6.53913849334999,2.08195256996599,8.06309502075624));
#21118=CARTESIAN_POINT('Ctrl Pts',(4.1319692288183,2.34484129441906,8.18992229426447));
#21119=CARTESIAN_POINT('Ctrl Pts',(2.60282100690976,0.467268375732359,8.31674956777266));
#21120=CARTESIAN_POINT('Ctrl Pts',(3.34755934886763,-1.83684515262515,8.44357684128091));
#21121=CARTESIAN_POINT('Ctrl Pts',(5.6863583496614,-2.46421552445023,8.57040411478909));
#21122=CARTESIAN_POINT('Ctrl Pts',(7.48427200499913,-0.842154848177517,
8.69723138829734));
#21123=CARTESIAN_POINT('Ctrl Pts',(7.1000953318101,1.54865728021659,8.82405866180553));
#21124=CARTESIAN_POINT('Ctrl Pts',(4.88451962637846,2.52579526592709,8.95088593531377));
#21125=CARTESIAN_POINT('Ctrl Pts',(2.86000791265811,1.19728983853755,9.07771320882196));
#21126=CARTESIAN_POINT('Ctrl Pts',(2.87461262793382,-1.22414796811865,9.20454048233019));
#21127=CARTESIAN_POINT('Ctrl Pts',(4.91500202445447,-2.52813625819363,9.33136775583841));
#21128=CARTESIAN_POINT('Ctrl Pts',(7.11862990299495,-1.52434418680528,9.45819502934663));
#21129=CARTESIAN_POINT('Ctrl Pts',(7.47393967750512,0.870928096569864,9.58502230285483));
#21130=CARTESIAN_POINT('Ctrl Pts',(5.65659087045061,2.47118359715601,9.71184957636306));
#21131=CARTESIAN_POINT('Ctrl Pts',(3.32552962272182,1.81564732180891,9.83867684987128));
#21132=CARTESIAN_POINT('Ctrl Pts',(2.60863861676512,-0.497281907856358,
9.9655041233795));
#21133=CARTESIAN_POINT('Ctrl Pts',(4.16032363855547,-2.35627302488586,10.0923313968877));
#21134=CARTESIAN_POINT('Ctrl Pts',(6.56414669812838,-2.06436715934487,10.2191586703959));
#21135=CARTESIAN_POINT('Ctrl Pts',(7.62580533546022,0.111972704871926,10.3459859439041));
#21136=CARTESIAN_POINT('Ctrl Pts',(6.37617653835352,2.18609961499206,10.4728132174123));
#21137=CARTESIAN_POINT('Ctrl Pts',(3.95596976227508,2.26467031333847,10.5996404909206));
#21138=CARTESIAN_POINT('Ctrl Pts',(2.57444306730565,0.275962726959528,10.7264677644287));
#21139=CARTESIAN_POINT('Ctrl Pts',(3.49270754449826,-1.96465465498572,10.853295037937));
#21140=CARTESIAN_POINT('Ctrl Pts',(5.87253555792415,-2.4118587352882,10.9801223114452));
#21141=CARTESIAN_POINT('Ctrl Pts',(7.54152895437427,-0.657426395247666,
11.1069495849534));
#21142=CARTESIAN_POINT('Ctrl Pts',(6.97616477246841,1.69713266770127,11.2337768584616));
#21143=CARTESIAN_POINT('Ctrl Pts',(4.69253186410977,2.50247869770875,11.3606041319699));
#21144=CARTESIAN_POINT('Ctrl Pts',(2.77521353452516,1.02347477075997,11.487431405478));
#21145=CARTESIAN_POINT('Ctrl Pts',(2.97442141226926,-1.38981394464989,11.6142586789863));
#21146=CARTESIAN_POINT('Ctrl Pts',(5.10829285501715,-2.53439348430674,11.7410859524945));
#21147=CARTESIAN_POINT('Ctrl Pts',(7.22898193815433,-1.36554437881099,11.8679132260027));
#21148=CARTESIAN_POINT('Ctrl Pts',(7.40057647709575,1.04994741641743,11.9947404995109));
#21149=CARTESIAN_POINT('Ctrl Pts',(5.46656281321151,2.50677603303065,12.1215677730191));
#21150=CARTESIAN_POINT('Ctrl Pts',(3.19214616311474,1.67576216864776,12.2483950465273));
#21151=CARTESIAN_POINT('Ctrl Pts',(2.6539536073717,-0.685789666746076,12.3752223200356));
#21152=CARTESIAN_POINT('Ctrl Pts',(4.34240679129502,-2.41972685250515,12.5020495935438));
#21153=CARTESIAN_POINT('Ctrl Pts',(6.71786699323475,-1.94792347258894,12.628876867052));
#21154=CARTESIAN_POINT('Ctrl Pts',(7.60873538465635,0.30816858502228,12.7557041405602));
#21155=CARTESIAN_POINT('Ctrl Pts',(6.67516509623461,1.6153592726669,12.8402556562324));
#21156=CARTESIAN_POINT('Ctrl Pts',(6.03504683094217,1.92787528928025,12.8825314140684));
#21157=CARTESIAN_POINT('Ctrl Pts',(3.93619209326963,1.62013485752469,-5.29165115932106));
#21158=CARTESIAN_POINT('Ctrl Pts',(3.39801758519098,1.23561895980355,-5.24935810060285));
#21159=CARTESIAN_POINT('Ctrl Pts',(2.74435052809542,-0.104854358212967,
-5.16478928404856));
#21160=CARTESIAN_POINT('Ctrl Pts',(3.90724889698388,-2.03294598783264,-5.03794470965818));
#21161=CARTESIAN_POINT('Ctrl Pts',(6.15412363201007,-2.09907083275189,-4.91111743614997));
#21162=CARTESIAN_POINT('Ctrl Pts',(7.43260302757121,-0.252067946212096,
-4.78429016264175));
#21163=CARTESIAN_POINT('Ctrl Pts',(6.57642845269443,1.82658316797167,-4.65746288913354));
#21164=CARTESIAN_POINT('Ctrl Pts',(4.36673595209344,2.23704641776749,-4.53063561562533));
#21165=CARTESIAN_POINT('Ctrl Pts',(2.82083503220571,0.605873504750498,-4.4038083421171));
#21166=CARTESIAN_POINT('Ctrl Pts',(3.34976986464268,-1.57858780666272,-4.2769810686089));
#21167=CARTESIAN_POINT('Ctrl Pts',(5.47076808588375,-2.32193582399472,-4.15015379510067));
#21168=CARTESIAN_POINT('Ctrl Pts',(7.24766927618217,-0.94579282806317,-4.02332652159245));
#21169=CARTESIAN_POINT('Ctrl Pts',(7.05846591074198,1.29373872094169,-3.89649924808424));
#21170=CARTESIAN_POINT('Ctrl Pts',(5.07586147957067,2.35227864510194,-3.76967197457603));
#21171=CARTESIAN_POINT('Ctrl Pts',(3.10965837295569,1.26357674007712,-3.6428447010678));
#21172=CARTESIAN_POINT('Ctrl Pts',(2.95468029882081,-0.97857146626037,-3.51601742755959));
#21173=CARTESIAN_POINT('Ctrl Pts',(4.75239847576922,-2.32743940941681,-3.38919015405137));
#21174=CARTESIAN_POINT('Ctrl Pts',(6.86178570453861,-1.55173211123067,-3.26236288054317));
#21175=CARTESIAN_POINT('Ctrl Pts',(7.35731224607869,0.640456830974584,-3.13553560703494));
#21176=CARTESIAN_POINT('Ctrl Pts',(5.78664216534575,2.24801170127096,-3.00870833352674));
#21177=CARTESIAN_POINT('Ctrl Pts',(3.58354383398488,1.80349490513657,-2.8818810600185));
#21178=CARTESIAN_POINT('Ctrl Pts',(2.75909039741521,-0.28732175223075,-2.7550537865103));
#21179=CARTESIAN_POINT('Ctrl Pts',(4.0658748021519,-2.11585997230547,-2.62822651300207));
#21180=CARTESIAN_POINT('Ctrl Pts',(6.31101378865387,-2.01295956559857,-2.50139923949386));
#21181=CARTESIAN_POINT('Ctrl Pts',(7.44505783611255,-0.0725519541120768,
-2.37457196598564));
#21182=CARTESIAN_POINT('Ctrl Pts',(6.43280776074269,1.93408387411994,-2.24774469247742));
#21183=CARTESIAN_POINT('Ctrl Pts',(4.19828450562832,2.17521329137638,-2.12091741896921));
#21184=CARTESIAN_POINT('Ctrl Pts',(2.78124714837218,0.430724052171207,-1.99409014546099));
#21185=CARTESIAN_POINT('Ctrl Pts',(3.47522208609301,-1.70694672649373,-1.86726287195277));
#21186=CARTESIAN_POINT('Ctrl Pts',(5.64672220829838,-2.28645064656837,-1.74043559844456));
#21187=CARTESIAN_POINT('Ctrl Pts',(7.31351838487148,-0.778794160413069,
-1.61360832493634));
#21188=CARTESIAN_POINT('Ctrl Pts',(6.95409472833523,1.43977569624093,-1.48678105142812));
#21189=CARTESIAN_POINT('Ctrl Pts',(4.89654702597431,2.34406272289244,-1.35995377791991));
#21190=CARTESIAN_POINT('Ctrl Pts',(3.01908424069936,1.10859881650414,-1.23312650441169));
#21191=CARTESIAN_POINT('Ctrl Pts',(3.03552687195881,-1.1388368808754,-1.10629923090347));
#21192=CARTESIAN_POINT('Ctrl Pts',(4.93086545125642,-2.34669831492216,-0.979471957395263));
#21193=CARTESIAN_POINT('Ctrl Pts',(6.97496176437862,-1.41240294582864,-0.852644683887045));
#21194=CARTESIAN_POINT('Ctrl Pts',(7.30188579570467,0.811188350196216,-0.725817410378829));
#21195=CARTESIAN_POINT('Ctrl Pts',(5.61320867035197,2.29429560873646,-0.598990136870612));
#21196=CARTESIAN_POINT('Ctrl Pts',(3.45042005035666,1.68308127706386,-0.472162863362396));
#21197=CARTESIAN_POINT('Ctrl Pts',(2.78779687051006,-0.464514610330093,
-0.34533558985418));
#21198=CARTESIAN_POINT('Ctrl Pts',(4.2302071462688,-2.18808363140476,-0.218508316345962));
#21199=CARTESIAN_POINT('Ctrl Pts',(6.46096310167163,-1.91428545490006,-0.0916810428377464));
#21200=CARTESIAN_POINT('Ctrl Pts',(7.44374459466541,0.106946375210275,0.0351462306704699));
#21201=CARTESIAN_POINT('Ctrl Pts',(6.28143074361666,2.03055342595704,0.161973504178687));
#21202=CARTESIAN_POINT('Ctrl Pts',(4.0350264964424,2.1005929312371,0.288800777686904));
#21203=CARTESIAN_POINT('Ctrl Pts',(2.75513635994022,0.253130127144199,0.415628051195119));
#21204=CARTESIAN_POINT('Ctrl Pts',(3.61009345376945,-1.82539962769057,0.542455324703337));
#21205=CARTESIAN_POINT('Ctrl Pts',(5.81945994180594,-2.23763414294083,0.669282598211551));
#21206=CARTESIAN_POINT('Ctrl Pts',(7.36644081343039,-0.607269841059064,
0.79610987171977));
#21207=CARTESIAN_POINT('Ctrl Pts',(6.83889221640734,1.5774338120256,0.922937145227985));
#21208=CARTESIAN_POINT('Ctrl Pts',(4.71838087318712,2.32219499340978,1.04976441873621));
#21209=CARTESIAN_POINT('Ctrl Pts',(2.9405913884407,0.947166949351214,1.17659169224442));
#21210=CARTESIAN_POINT('Ctrl Pts',(3.12835862554768,-1.29247164620201,1.30341896575264));
#21211=CARTESIAN_POINT('Ctrl Pts',(5.11028140276398,-2.35229223440248,1.43024623926085));
#21212=CARTESIAN_POINT('Ctrl Pts',(7.07718410790996,-1.26484967384501,1.55707351276907));
#21213=CARTESIAN_POINT('Ctrl Pts',(7.23360203035833,0.977196491504692,1.68390078627729));
#21214=CARTESIAN_POINT('Ctrl Pts',(5.43675085285186,2.32721998015813,1.8107280597855));
#21215=CARTESIAN_POINT('Ctrl Pts',(3.32686568769237,1.55286724150316,1.93755533329372));
#21216=CARTESIAN_POINT('Ctrl Pts',(2.82993115405241,-0.639002655023184,
2.06438260680194));
#21217=CARTESIAN_POINT('Ctrl Pts',(4.39956827564003,-2.24756626289093,2.19120988031016));
#21218=CARTESIAN_POINT('Ctrl Pts',(6.60295170073458,-1.80446463116177,2.31803715381837));
#21219=CARTESIAN_POINT('Ctrl Pts',(7.42874798951307,0.285821967240959,2.44486442732659));
#21220=CARTESIAN_POINT('Ctrl Pts',(6.12313841429284,2.11519924137433,2.5716917008348));
#21221=CARTESIAN_POINT('Ctrl Pts',(3.87793379115134,2.01374100244589,2.69851897434302));
#21222=CARTESIAN_POINT('Ctrl Pts',(2.7426435637642,0.0740622471820766,2.82534624785124));
#21223=CARTESIAN_POINT('Ctrl Pts',(3.75360447327307,-1.93322338607179,2.95217352135945));
#21224=CARTESIAN_POINT('Ctrl Pts',(5.98797237893932,-2.17578809115262,3.07900079486767));
#21225=CARTESIAN_POINT('Ctrl Pts',(7.40613001109016,-0.432209442397493,
3.20582806837589));
#21226=CARTESIAN_POINT('Ctrl Pts',(6.71352834298829,1.70590666842646,3.3326553418841));
#21227=CARTESIAN_POINT('Ctrl Pts',(4.54240091132322,2.28680532524515,3.45948261539232));
#21228=CARTESIAN_POINT('Ctrl Pts',(2.8746366400517,0.780219811743623,3.58630988890054));
#21229=CARTESIAN_POINT('Ctrl Pts',(3.23263513078033,-1.43858046197604,3.71313716240875));
#21230=CARTESIAN_POINT('Ctrl Pts',(5.28960154262576,-2.34418896158393,3.83996443591697));
#21231=CARTESIAN_POINT('Ctrl Pts',(7.16785753707561,-1.10993129264456,3.96679170942518));
#21232=CARTESIAN_POINT('Ctrl Pts',(7.15285854274059,1.13751450296238,4.09361898293341));
#21233=CARTESIAN_POINT('Ctrl Pts',(5.25829622060271,2.3465931528268,4.22044625644161));
#21234=CARTESIAN_POINT('Ctrl Pts',(3.2136001873802,1.41361099557698,4.34727352994984));
#21235=CARTESIAN_POINT('Ctrl Pts',(2.88524790634857,-0.809769843047783,
4.47410080345805));
#21236=CARTESIAN_POINT('Ctrl Pts',(4.57297201385219,-2.2939615122649,4.60092807696627));
#21237=CARTESIAN_POINT('Ctrl Pts',(6.73615279933309,-1.68413656742527,4.72775535047449));
#21238=CARTESIAN_POINT('Ctrl Pts',(7.40015534420757,0.463033242911717,4.8545826239827));
#21239=CARTESIAN_POINT('Ctrl Pts',(5.95885249537868,2.18752843628864,4.98140989749092));
#21240=CARTESIAN_POINT('Ctrl Pts',(3.7279211267601,1.91516323561854,5.10823717099913));
#21241=CARTESIAN_POINT('Ctrl Pts',(2.74384150435911,-0.105436890778946,
5.23506444450736));
#21242=CARTESIAN_POINT('Ctrl Pts',(3.90491949243924,-2.02979015346703,5.36189171801556));
#21243=CARTESIAN_POINT('Ctrl Pts',(6.15127828650479,-2.10127261527921,5.48871899152379));
#21244=CARTESIAN_POINT('Ctrl Pts',(7.43235487111032,-0.25463232588935,5.61554626503199));
#21245=CARTESIAN_POINT('Ctrl Pts',(6.5787330909715,1.82444617924099,5.74237353854023));
#21246=CARTESIAN_POINT('Ctrl Pts',(4.36963185633347,2.23809978933421,5.86920081204843));
#21247=CARTESIAN_POINT('Ctrl Pts',(2.82160404427482,0.608729522293797,5.99602808555666));
#21248=CARTESIAN_POINT('Ctrl Pts',(3.34774919467065,-1.57631254932345,6.12285535906485));
#21249=CARTESIAN_POINT('Ctrl Pts',(5.46778170532425,-2.32243568111486,6.2496826325731));
#21250=CARTESIAN_POINT('Ctrl Pts',(7.2464540684141,-0.948549878435926,6.37650990608129));
#21251=CARTESIAN_POINT('Ctrl Pts',(7.06012549513016,1.2912088667865,6.50333717958953));
#21252=CARTESIAN_POINT('Ctrl Pts',(5.07888389934713,2.35230231844925,6.63016445309772));
#21253=CARTESIAN_POINT('Ctrl Pts',(3.11128308453918,1.26612341624693,6.75699172660596));
#21254=CARTESIAN_POINT('Ctrl Pts',(2.95342502277967,-0.975821811977877,
6.88381900011415));
#21255=CARTESIAN_POINT('Ctrl Pts',(4.74940864607765,-2.32699922404035,7.01064627362239));
#21256=CARTESIAN_POINT('Ctrl Pts',(6.85979077909989,-1.55400192349981,7.13747354713059));
#21257=CARTESIAN_POINT('Ctrl Pts',(7.35813315122608,0.637548316436762,7.26430082063883));
#21258=CARTESIAN_POINT('Ctrl Pts',(5.78952960943609,2.24711984411309,7.39112809414702));
#21259=CARTESIAN_POINT('Ctrl Pts',(3.58586201391573,1.80543364048445,7.51795536765526));
#21260=CARTESIAN_POINT('Ctrl Pts',(2.75872320622145,-0.284322078930742,
7.64478264116346));
#21261=CARTESIAN_POINT('Ctrl Pts',(4.06315741712276,-2.11453763002099,7.77160991467167));
#21262=CARTESIAN_POINT('Ctrl Pts',(6.30842674846097,-2.01452161243064,7.89843718817991));
#21263=CARTESIAN_POINT('Ctrl Pts',(7.44496268842068,-0.0755725075796159,
8.0252644616881));
#21264=CARTESIAN_POINT('Ctrl Pts',(6.4352913613404,1.93236209924735,8.15209173519635));
#21265=CARTESIAN_POINT('Ctrl Pts',(4.20107972734041,2.17636199376026,8.27891900870454));
#21266=CARTESIAN_POINT('Ctrl Pts',(2.78180240528509,0.433694653983792,8.40574628221277));
#21267=CARTESIAN_POINT('Ctrl Pts',(3.47303051807501,-1.7048659063242,8.53257355572097));
#21268=CARTESIAN_POINT('Ctrl Pts',(5.64378436332965,-2.28715906044984,8.6594008292292));
#21269=CARTESIAN_POINT('Ctrl Pts',(7.31251604118465,-0.781645141100505,
8.78622810273741));
#21270=CARTESIAN_POINT('Ctrl Pts',(6.95594286396882,1.43738463410957,8.91305537624562));
#21271=CARTESIAN_POINT('Ctrl Pts',(4.89955859136301,2.34431423306421,9.03988264975386));
#21272=CARTESIAN_POINT('Ctrl Pts',(3.02051016273363,1.11126331078796,9.16670992326206));
#21273=CARTESIAN_POINT('Ctrl Pts',(3.03406551393433,-1.13619165565418,9.29353719677028));
#21274=CARTESIAN_POINT('Ctrl Pts',(4.92785079724033,-2.34648702258678,9.42036447027849));
#21275=CARTESIAN_POINT('Ctrl Pts',(6.9731457068194,-1.4148184619012,9.54719174378672));
#21276=CARTESIAN_POINT('Ctrl Pts',(7.30292610223287,0.808351001487389,9.67401901729492));
#21277=CARTESIAN_POINT('Ctrl Pts',(5.61615570864899,2.29362646984029,9.80084629080315));
#21278=CARTESIAN_POINT('Ctrl Pts',(3.45258365080479,1.68519116183362,9.92767356431137));
#21279=CARTESIAN_POINT('Ctrl Pts',(2.78720201378478,-0.461551682418371,
10.0545008378195));
#21280=CARTESIAN_POINT('Ctrl Pts',(4.22739684306776,-2.1869723424308,10.1813281113278));
#21281=CARTESIAN_POINT('Ctrl Pts',(6.45850270043673,-1.91604021878082,10.308155384836));
#21282=CARTESIAN_POINT('Ctrl Pts',(7.44388005375085,0.103927348858032,10.4349826583442));
#21283=CARTESIAN_POINT('Ctrl Pts',(6.28403839333469,2.02902607010827,10.5618099318524));
#21284=CARTESIAN_POINT('Ctrl Pts',(4.03772600663513,2.10195138156167,10.6886372053606));
#21285=CARTESIAN_POINT('Ctrl Pts',(2.75546345033636,0.25613451625857,10.8154644788688));
#21286=CARTESIAN_POINT('Ctrl Pts',(3.60774966396572,-1.82349216219961,10.9422917523771));
#21287=CARTESIAN_POINT('Ctrl Pts',(5.81658454436188,-2.23856416137554,11.0691190258853));
#21288=CARTESIAN_POINT('Ctrl Pts',(7.3656590188332,-0.61018962081453,11.1959462993935));
#21289=CARTESIAN_POINT('Ctrl Pts',(6.84091684499746,1.57519190963801,11.3227735729017));
#21290=CARTESIAN_POINT('Ctrl Pts',(4.72136535071037,2.32267298467096,11.4496008464099));
#21291=CARTESIAN_POINT('Ctrl Pts',(2.94180834939884,0.94993703751125,11.5764281199182));
#21292=CARTESIAN_POINT('Ctrl Pts',(3.12670293267481,-1.28995435841787,11.7032553934263));
#21293=CARTESIAN_POINT('Ctrl Pts',(5.1072534793665,-2.35229466045606,11.8300826669346));
#21294=CARTESIAN_POINT('Ctrl Pts',(7.07556883277958,-1.26742858628029,11.9569099404428));
#21295=CARTESIAN_POINT('Ctrl Pts',(7.2348341245406,0.97450759587711,12.083737213951));
#21296=CARTESIAN_POINT('Ctrl Pts',(5.43978136616892,2.32666155195322,12.2105644874592));
#21297=CARTESIAN_POINT('Ctrl Pts',(3.32878393234366,1.5553569033037,12.3373917609675));
#21298=CARTESIAN_POINT('Ctrl Pts',(2.8292610748984,-0.636514961576311,12.4642190344756));
#21299=CARTESIAN_POINT('Ctrl Pts',(4.39639713075019,-2.24586694613722,12.5910463079839));
#21300=CARTESIAN_POINT('Ctrl Pts',(6.60117803148594,-1.80796313276562,12.7178735814921));
#21301=CARTESIAN_POINT('Ctrl Pts',(7.42803659677434,0.28602634971914,12.8447008550003));
#21302=CARTESIAN_POINT('Ctrl Pts',(6.56154431046876,1.49929401860499,12.9292523706725));
#21303=CARTESIAN_POINT('Ctrl Pts',(5.96741921236085,1.7893554324062,12.9715281285085));
#21304=CARTESIAN_POINT('',(6.25533271652633,-1.62367300596587,12.7072733567685));
#21305=CARTESIAN_POINT('Ctrl Pts',(6.25666084923699,-1.62473234417576,12.7063625311661));
#21306=CARTESIAN_POINT('Ctrl Pts',(6.30032205070727,-1.60059242823093,12.7063625311661));
#21307=CARTESIAN_POINT('Ctrl Pts',(6.34291068770113,-1.57476837059284,12.7063625311661));
#21308=CARTESIAN_POINT('Ctrl Pts',(6.38431766016846,-1.54728798228453,12.7063625311661));
#21309=CARTESIAN_POINT('Ctrl Pts',(6.44363247708358,-1.50792277144838,12.7063625311661));
#21310=CARTESIAN_POINT('Ctrl Pts',(6.50052383028944,-1.46516132071873,12.7063625311661));
#21311=CARTESIAN_POINT('Ctrl Pts',(6.55492121660405,-1.41935664268984,12.7063625311661));
#21312=CARTESIAN_POINT('Ctrl Pts',(6.61105831717652,-1.37208705877406,12.7063625311661));
#21313=CARTESIAN_POINT('Ctrl Pts',(6.66453998122585,-1.32157607379915,12.7063625311661));
#21314=CARTESIAN_POINT('Ctrl Pts',(6.71526745766364,-1.26816023566171,12.7063625311661));
#21315=CARTESIAN_POINT('Ctrl Pts',(6.74038993745235,-1.24170636079468,12.7063625311661));
#21316=CARTESIAN_POINT('Ctrl Pts',(6.76483652651217,-1.21453928084961,12.706362531166));
#21317=CARTESIAN_POINT('Ctrl Pts',(6.78859267017858,-1.18669594610846,12.706362531166));
#21318=CARTESIAN_POINT('Ctrl Pts',(6.80262589826627,-1.17024833269817,12.706362531166));
#21319=CARTESIAN_POINT('Ctrl Pts',(6.81641816076635,-1.1535646942934,12.7063625311661));
#21320=CARTESIAN_POINT('Ctrl Pts',(6.82996613291959,-1.13665228404755,12.7063625311661));
#21321=CARTESIAN_POINT('Ctrl Pts',(6.84137015391622,-1.122416243453,12.7063625311661));
#21322=CARTESIAN_POINT('Ctrl Pts',(6.85260488848684,-1.10801285918862,12.7063625311661));
#21323=CARTESIAN_POINT('Ctrl Pts',(6.86364697729733,-1.09347496824222,12.7063625311661));
#21324=CARTESIAN_POINT('Ctrl Pts',(6.90963170604025,-1.03293198736804,12.7063625311661));
#21325=CARTESIAN_POINT('Ctrl Pts',(6.95233668874753,-0.96999049639788,12.706362531166));
#21326=CARTESIAN_POINT('Ctrl Pts',(6.99167813852895,-0.905029924872353,
12.706362531166));
#21327=CARTESIAN_POINT('Ctrl Pts',(7.03205889091705,-0.838353257684557,
12.706362531166));
#21328=CARTESIAN_POINT('Ctrl Pts',(7.06889673727258,-0.769548784540488,
12.706362531166));
#21329=CARTESIAN_POINT('Ctrl Pts',(7.10207071012869,-0.698980285508197,
12.706362531166));
#21330=CARTESIAN_POINT('Ctrl Pts',(7.135188177495,-0.628531986357274,12.706362531166));
#21331=CARTESIAN_POINT('Ctrl Pts',(7.16465482357667,-0.556324770439544,
12.706362531166));
#21332=CARTESIAN_POINT('Ctrl Pts',(7.19031105018904,-0.482686730203765,
12.706362531166));
#21333=CARTESIAN_POINT('Ctrl Pts',(7.19984472032834,-0.455323361618091,
12.706362531166));
#21334=CARTESIAN_POINT('Ctrl Pts',(7.20885180882894,-0.427762155343313,
12.706362531166));
#21335=CARTESIAN_POINT('Ctrl Pts',(7.21732248911392,-0.400019139505833,
12.706362531166));
#21336=CARTESIAN_POINT('Ctrl Pts',(7.22131145096394,-0.386954565226427,
12.706362531166));
#21337=CARTESIAN_POINT('Ctrl Pts',(7.2251817406524,-0.373848315982475,12.706362531166));
#21338=CARTESIAN_POINT('Ctrl Pts',(7.22892749257759,-0.360719691257243,
12.706362531166));
#21339=CARTESIAN_POINT('Ctrl Pts',(7.25098092868138,-0.283423785844427,
12.706362531166));
#21340=CARTESIAN_POINT('Ctrl Pts',(7.26876312114318,-0.20521987500682,12.706362531166));
#21341=CARTESIAN_POINT('Ctrl Pts',(7.28215780080698,-0.126489502252328,
12.706362531166));
#21342=CARTESIAN_POINT('Ctrl Pts',(7.29550082974256,-0.0480627187725307,
12.706362531166));
#21343=CARTESIAN_POINT('Ctrl Pts',(7.30449066516009,0.0308874283709469,
12.706362531166));
#21344=CARTESIAN_POINT('Ctrl Pts',(7.30897015665432,0.110012229383381,12.706362531166));
#21345=CARTESIAN_POINT('Ctrl Pts',(7.31197287395277,0.163051599821535,12.706362531166));
#21346=CARTESIAN_POINT('Ctrl Pts',(7.312948053959,0.216170020118987,12.706362531166));
#21347=CARTESIAN_POINT('Ctrl Pts',(7.31183578929012,0.269266404483285,12.706362531166));
#21348=CARTESIAN_POINT('Ctrl Pts',(7.31082231252311,0.317646932491655,12.706362531166));
#21349=CARTESIAN_POINT('Ctrl Pts',(7.30807561817696,0.366009266789958,12.706362531166));
#21350=CARTESIAN_POINT('Ctrl Pts',(7.30364204599346,0.414293597553426,12.706362531166));
#21351=CARTESIAN_POINT('Ctrl Pts',(7.30239041935636,0.42792458223954,12.706362531166));
#21352=CARTESIAN_POINT('Ctrl Pts',(7.30100430601789,0.441549350536377,12.706362531166));
#21353=CARTESIAN_POINT('Ctrl Pts',(7.29948463756176,0.455166553839244,12.706362531166));
#21354=CARTESIAN_POINT('Ctrl Pts',(7.29800012491074,0.468468738597494,12.706362531166));
#21355=CARTESIAN_POINT('Ctrl Pts',(7.29638902328974,0.481755694243806,12.706362531166));
#21356=CARTESIAN_POINT('Ctrl Pts',(7.29465345449701,0.495020590754398,12.706362531166));
#21357=CARTESIAN_POINT('Ctrl Pts',(7.28453102028643,0.572386030142982,12.706362531166));
#21358=CARTESIAN_POINT('Ctrl Pts',(7.27017225257139,0.649059725150864,12.706362531166));
#21359=CARTESIAN_POINT('Ctrl Pts',(7.2518463038517,0.724789641219328,12.706362531166));
#21360=CARTESIAN_POINT('Ctrl Pts',(7.23298733911895,0.802722185842006,12.706362531166));
#21361=CARTESIAN_POINT('Ctrl Pts',(7.20992700069116,0.879655964123195,12.7063625311661));
#21362=CARTESIAN_POINT('Ctrl Pts',(7.18290443834463,0.955323585080013,12.7063625311661));
#21363=CARTESIAN_POINT('Ctrl Pts',(7.15535953714381,1.03245384077628,12.706362531166));
#21364=CARTESIAN_POINT('Ctrl Pts',(7.12369756612586,1.10826938256074,12.7063625311661));
#21365=CARTESIAN_POINT('Ctrl Pts',(7.08811837296769,1.18248233643891,12.7063625311661));
#21366=CARTESIAN_POINT('Ctrl Pts',(7.07816689635174,1.20323965018226,12.7063625311661));
#21367=CARTESIAN_POINT('Ctrl Pts',(7.06790866277265,1.22387151865158,12.7063625311661));
#21368=CARTESIAN_POINT('Ctrl Pts',(7.05734735003915,1.24437143188873,12.7063625311661));
#21369=CARTESIAN_POINT('Ctrl Pts',(7.04849952500069,1.26154539976591,12.7063625311661));
#21370=CARTESIAN_POINT('Ctrl Pts',(7.03943898195409,1.27862675491862,12.7063625311661));
#21371=CARTESIAN_POINT('Ctrl Pts',(7.03016772806532,1.29561159813897,12.7063625311661));
#21372=CARTESIAN_POINT('Ctrl Pts',(7.02341966037244,1.30797398980452,12.7063625311661));
#21373=CARTESIAN_POINT('Ctrl Pts',(7.01656466503568,1.32027661892001,12.7063625311661));
#21374=CARTESIAN_POINT('Ctrl Pts',(7.00960470932485,1.33251686759166,12.7063625311661));
#21375=CARTESIAN_POINT('Ctrl Pts',(6.96795839788621,1.40575888657079,12.7063625311661));
#21376=CARTESIAN_POINT('Ctrl Pts',(6.9225501456431,1.47678283374337,12.7063625311661));
#21377=CARTESIAN_POINT('Ctrl Pts',(6.87362331348931,1.54529429041433,12.7063625311661));
#21378=CARTESIAN_POINT('Ctrl Pts',(6.82436351863789,1.61427198939912,12.7063625311661));
#21379=CARTESIAN_POINT('Ctrl Pts',(6.77153672791292,1.68070382107673,12.7063625311661));
#21380=CARTESIAN_POINT('Ctrl Pts',(6.71534151108349,1.74427364312724,12.7063625311661));
#21381=CARTESIAN_POINT('Ctrl Pts',(6.69873238379939,1.76306241778523,12.7063625311661));
#21382=CARTESIAN_POINT('Ctrl Pts',(6.68182869401359,1.7816010220568,12.7063625311661));
#21383=CARTESIAN_POINT('Ctrl Pts',(6.66463481673223,1.79988084526421,12.7063625311661));
#21384=CARTESIAN_POINT('Ctrl Pts',(6.65367857690042,1.81152906886533,12.7063625311661));
#21385=CARTESIAN_POINT('Ctrl Pts',(6.64261103852896,1.82306524299457,12.7063625311661));
#21386=CARTESIAN_POINT('Ctrl Pts',(6.63143491401651,1.8344862619574,12.7063625311661));
#21387=CARTESIAN_POINT('Ctrl Pts',(6.57115803581338,1.89608394442874,12.7063625311661));
#21388=CARTESIAN_POINT('Ctrl Pts',(6.50771572710583,1.95434495315579,12.7063625311661));
#21389=CARTESIAN_POINT('Ctrl Pts',(6.4413306123096,2.00895641381313,12.7063625311661));
#21390=CARTESIAN_POINT('Ctrl Pts',(6.37554842109209,2.0630718816956,12.7063625311661));
#21391=CARTESIAN_POINT('Ctrl Pts',(6.30687613262566,2.11360466634069,12.7063625311661));
#21392=CARTESIAN_POINT('Ctrl Pts',(6.23548856958003,2.16022201180838,12.7063625311661));
#21393=CARTESIAN_POINT('Ctrl Pts',(6.21355277048793,2.17454647787444,12.7063625311661));
#21394=CARTESIAN_POINT('Ctrl Pts',(6.19136032543429,2.1885009958289,12.7063625311661));
#21395=CARTESIAN_POINT('Ctrl Pts',(6.16891561580437,2.2020751695661,12.7063625311661));
#21396=CARTESIAN_POINT('Ctrl Pts',(6.2322445509742,-1.63799676314545,12.7063625311661));
#21397=CARTESIAN_POINT('Ctrl Pts',(6.23966578565302,-1.63283896134468,12.7066661397002));
#21398=CARTESIAN_POINT('Ctrl Pts',(6.24705196728502,-1.62763072394165,12.7069697482344));
#21399=CARTESIAN_POINT('Ctrl Pts',(6.25440241361523,-1.62237253201659,12.7072733567685));
#21400=CARTESIAN_POINT('Ctrl Pts',(4.0161764580452,-2.20524422515229,-5.29363746883395));
#21401=CARTESIAN_POINT('Ctrl Pts',(3.96415957839439,-2.17411111039703,-5.29363746883395));
#21402=CARTESIAN_POINT('Ctrl Pts',(3.91346144812925,-2.14096669141098,-5.29363746883395));
#21403=CARTESIAN_POINT('Ctrl Pts',(3.86421540032617,-2.10580418894025,-5.29363746883395));
#21404=CARTESIAN_POINT('Ctrl Pts',(3.7946109321332,-2.05610543352749,-5.29363746883395));
#21405=CARTESIAN_POINT('Ctrl Pts',(3.72790538661327,-2.00237606934197,-5.29363746883395));
#21406=CARTESIAN_POINT('Ctrl Pts',(3.66426959291209,-1.94498134030856,-5.29363746883395));
#21407=CARTESIAN_POINT('Ctrl Pts',(3.63249149466555,-1.91631987115769,-5.29363746883395));
#21408=CARTESIAN_POINT('Ctrl Pts',(3.60147957008092,-1.88674383400354,-5.29363746883395));
#21409=CARTESIAN_POINT('Ctrl Pts',(3.57125926033597,-1.85629625244888,-5.29363746883395));
#21410=CARTESIAN_POINT('Ctrl Pts',(3.55712156398471,-1.84205223356612,-5.29363746883395));
#21411=CARTESIAN_POINT('Ctrl Pts',(3.54315715919797,-1.82761745310723,-5.29363746883395));
#21412=CARTESIAN_POINT('Ctrl Pts',(3.52936887534993,-1.81299623318088,-5.29363746883395));
#21413=CARTESIAN_POINT('Ctrl Pts',(3.51960577775136,-1.80264335687485,-5.29363746883395));
#21414=CARTESIAN_POINT('Ctrl Pts',(3.50993238971118,-1.79219841760079,-5.29363746883395));
#21415=CARTESIAN_POINT('Ctrl Pts',(3.5003555839824,-1.7816697380745,-5.29363746883395));
#21416=CARTESIAN_POINT('Ctrl Pts',(3.443365838096,-1.71901557261304,-5.29363746883395));
#21417=CARTESIAN_POINT('Ctrl Pts',(3.38973035102999,-1.65333255407641,-5.29363746883395));
#21418=CARTESIAN_POINT('Ctrl Pts',(3.3396145347394,-1.58497710192186,-5.29363746883395));
#21419=CARTESIAN_POINT('Ctrl Pts',(3.28953311945874,-1.51666857101419,-5.29363746883395));
#21420=CARTESIAN_POINT('Ctrl Pts',(3.24296617947589,-1.44569027005333,-5.29363746883395));
#21421=CARTESIAN_POINT('Ctrl Pts',(3.20012684269656,-1.37237966206277,-5.29363746883395));
#21422=CARTESIAN_POINT('Ctrl Pts',(3.19379617350613,-1.36154603945727,-5.29363746883395));
#21423=CARTESIAN_POINT('Ctrl Pts',(3.18754699922928,-1.35066146707165,-5.29363746883395));
#21424=CARTESIAN_POINT('Ctrl Pts',(3.1813801042914,-1.33972702074568,-5.29363746883395));
#21425=CARTESIAN_POINT('Ctrl Pts',(3.17376606231537,-1.32622665562688,-5.29363746883395));
#21426=CARTESIAN_POINT('Ctrl Pts',(3.1662774447426,-1.31265026282385,-5.29363746883395));
#21427=CARTESIAN_POINT('Ctrl Pts',(3.15891578258334,-1.29899986614287,-5.29363746883395));
#21428=CARTESIAN_POINT('Ctrl Pts',(3.15231892098481,-1.28676760449851,-5.29363746883395));
#21429=CARTESIAN_POINT('Ctrl Pts',(3.14582890907765,-1.27448500477395,-5.29363746883395));
#21430=CARTESIAN_POINT('Ctrl Pts',(3.13944646896944,-1.26215385852175,-5.29363746883395));
#21431=CARTESIAN_POINT('Ctrl Pts',(3.10127090708007,-1.1883970462467,-5.29363746883395));
#21432=CARTESIAN_POINT('Ctrl Pts',(3.06693869563808,-1.11290254769809,-5.29363746883394));
#21433=CARTESIAN_POINT('Ctrl Pts',(3.03661028899585,-1.03600109297847,-5.29363746883395));
#21434=CARTESIAN_POINT('Ctrl Pts',(3.00661636168852,-0.959947752297,-5.29363746883395));
#21435=CARTESIAN_POINT('Ctrl Pts',(2.98053819156754,-0.882517366186935,
-5.29363746883395));
#21436=CARTESIAN_POINT('Ctrl Pts',(2.95858073793476,-0.804021262619071,
-5.29363746883395));
#21437=CARTESIAN_POINT('Ctrl Pts',(2.9372611370858,-0.727805430662714,-5.29363746883395));
#21438=CARTESIAN_POINT('Ctrl Pts',(2.91982628590018,-0.650584114279385,
-5.29363746883395));
#21439=CARTESIAN_POINT('Ctrl Pts',(2.90651258241353,-0.572646792630231,
-5.29363746883395));
#21440=CARTESIAN_POINT('Ctrl Pts',(2.90242099371331,-0.54869496999091,-5.29363746883395));
#21441=CARTESIAN_POINT('Ctrl Pts',(2.89871899161892,-0.524675600344247,
-5.29363746883395));
#21442=CARTESIAN_POINT('Ctrl Pts',(2.89541441031052,-0.500597345162154,
-5.29363746883395));
#21443=CARTESIAN_POINT('Ctrl Pts',(2.89342273847487,-0.48608537580135,-5.29363746883395));
#21444=CARTESIAN_POINT('Ctrl Pts',(2.89157543776742,-0.471552019314399,
-5.29363746883395));
#21445=CARTESIAN_POINT('Ctrl Pts',(2.88987430653294,-0.456999201895081,
-5.29363746883395));
#21446=CARTESIAN_POINT('Ctrl Pts',(2.88843961385479,-0.444725709894666,
-5.29363746883395));
#21447=CARTESIAN_POINT('Ctrl Pts',(2.88710998374673,-0.432447681393096,
-5.29363746883395));
#21448=CARTESIAN_POINT('Ctrl Pts',(2.88588612845473,-0.420167265009195,
-5.29363746883395));
#21449=CARTESIAN_POINT('Ctrl Pts',(2.87814293320273,-0.342470447045378,
-5.29363746883395));
#21450=CARTESIAN_POINT('Ctrl Pts',(2.8746281056688,-0.264664011995165,-5.29363746883395));
#21451=CARTESIAN_POINT('Ctrl Pts',(2.8755201572915,-0.187027918273236,-5.29363746883395));
#21452=CARTESIAN_POINT('Ctrl Pts',(2.87584760148051,-0.1585301418004,-5.29363746883395));
#21453=CARTESIAN_POINT('Ctrl Pts',(2.87676932323159,-0.130055355239279,
-5.29363746883395));
#21454=CARTESIAN_POINT('Ctrl Pts',(2.87829591735836,-0.101617658814265,
-5.29363746883395));
#21455=CARTESIAN_POINT('Ctrl Pts',(2.88255816402082,-0.022219687506853,
-5.29363746883395));
#21456=CARTESIAN_POINT('Ctrl Pts',(2.89153207798952,0.0568907686398899,
-5.29363746883395));
#21457=CARTESIAN_POINT('Ctrl Pts',(2.9050288877662,0.135390588484381,-5.29363746883395));
#21458=CARTESIAN_POINT('Ctrl Pts',(2.91810519077797,0.211444667014056,-5.29363746883395));
#21459=CARTESIAN_POINT('Ctrl Pts',(2.93542774284134,0.286926220129041,-5.29363746883395));
#21460=CARTESIAN_POINT('Ctrl Pts',(2.95686365990608,0.361515460144451,-5.29363746883395));
#21461=CARTESIAN_POINT('Ctrl Pts',(2.9615370009577,0.377776997092935,-5.29363746883395));
#21462=CARTESIAN_POINT('Ctrl Pts',(2.96640746651885,0.394000351614356,-5.29363746883395));
#21463=CARTESIAN_POINT('Ctrl Pts',(2.97146478449135,0.410154161007378,-5.29363746883395));
#21464=CARTESIAN_POINT('Ctrl Pts',(2.99470377368125,0.484382873518835,-5.29363746883395));
#21465=CARTESIAN_POINT('Ctrl Pts',(3.02191236934093,0.557250909909585,-5.29363746883395));
#21466=CARTESIAN_POINT('Ctrl Pts',(3.05288579579963,0.628467523783645,-5.29363746883395));
#21467=CARTESIAN_POINT('Ctrl Pts',(3.08387954778233,0.699730871750787,-5.29363746883395));
#21468=CARTESIAN_POINT('Ctrl Pts',(3.11864373988791,0.769341465886313,-5.29363746883396));
#21469=CARTESIAN_POINT('Ctrl Pts',(3.15701609577644,0.836978638120724,-5.29363746883396));
#21470=CARTESIAN_POINT('Ctrl Pts',(3.19461969513807,0.903260758875702,-5.29363746883396));
#21471=CARTESIAN_POINT('Ctrl Pts',(3.23568904181845,0.967648362437176,-5.29363746883396));
#21472=CARTESIAN_POINT('Ctrl Pts',(3.28010225514524,1.0298008894447,-5.29363746883396));
#21473=CARTESIAN_POINT('Ctrl Pts',(3.29720451409011,1.05373405102749,-5.29363746883396));
#21474=CARTESIAN_POINT('Ctrl Pts',(3.31480287590974,1.07733533248401,-5.29363746883396));
#21475=CARTESIAN_POINT('Ctrl Pts',(3.33289130559999,1.10058341461658,-5.29363746883396));
#21476=CARTESIAN_POINT('Ctrl Pts',(3.34051062023558,1.11037610837029,-5.29363746883396));
#21477=CARTESIAN_POINT('Ctrl Pts',(3.34821707277534,1.12010621186302,-5.29363746883396));
#21478=CARTESIAN_POINT('Ctrl Pts',(3.3560008305098,1.12976079639403,-5.29363746883396));
#21479=CARTESIAN_POINT('Ctrl Pts',(3.40307483513459,1.18814904181068,-5.29363746883396));
#21480=CARTESIAN_POINT('Ctrl Pts',(3.45305491913425,1.24388420374776,-5.29363746883395));
#21481=CARTESIAN_POINT('Ctrl Pts',(3.50578778719035,1.29668117475663,-5.29363746883395));
#21482=CARTESIAN_POINT('Ctrl Pts',(3.55766743438001,1.34862388770958,-5.29363746883395));
#21483=CARTESIAN_POINT('Ctrl Pts',(3.6122121661761,1.39772327576028,-5.29363746883395));
#21484=CARTESIAN_POINT('Ctrl Pts',(3.66930278229164,1.44366593341478,-5.29363746883395));
#21485=CARTESIAN_POINT('Ctrl Pts',(3.72456640762552,1.48813835274063,-5.29363746883395));
#21486=CARTESIAN_POINT('Ctrl Pts',(3.78221616455222,1.52965316492833,-5.29363746883396));
#21487=CARTESIAN_POINT('Ctrl Pts',(3.84216013143835,1.56788041483154,-5.29363746883395));
#21488=CARTESIAN_POINT('Ctrl Pts',(3.87203299659095,1.58693083042519,-5.29363746883395));
#21489=CARTESIAN_POINT('Ctrl Pts',(3.90247582953994,1.60516403142193,-5.29363746883395));
#21490=CARTESIAN_POINT('Ctrl Pts',(3.93347817078402,1.62253437445171,-5.29363746883395));
#21491=CARTESIAN_POINT('Origin',(5.09382715545311,0.,12.7063625311661));
#21492=CARTESIAN_POINT('Origin',(1.8440744744562,0.,-5.29363746883395));
#21493=CARTESIAN_POINT('',(8.34357983645002,-3.97979921880339E-16,-5.29363746883395));
#21494=CARTESIAN_POINT('Origin',(5.09382715545311,0.,-5.29363746883395));
#21495=CARTESIAN_POINT('Origin',(5.09382715545311,0.,-5.79500850830927));
#21496=CARTESIAN_POINT('',(12.124643767714,-8.61026705959731E-16,-6.2963795477846));
#21497=CARTESIAN_POINT('Origin',(5.09382715545311,0.,-6.29637954778459));
#21498=CARTESIAN_POINT('',(10.234111802082,-6.29503313920035E-16,-5.79500850830927));
#21499=CARTESIAN_POINT('Origin',(5.09382715545311,0.,-10.2993262321375));
#21500=CARTESIAN_POINT('',(10.1694090836076,-6.21579516212456E-16,-14.3022729164904));
#21501=CARTESIAN_POINT('',(11.1470264256608,7.41303111086094E-16,-10.2993262321375));
#21502=CARTESIAN_POINT('Origin',(5.09382715545311,0.,-14.3022729164904));
#21503=CARTESIAN_POINT('Origin',(5.09382715545311,0.,-14.3022729164904));
#21504=CARTESIAN_POINT('',(0.,0.,0.));
#21505=CARTESIAN_POINT('Origin',(5.09382715545311,0.,-0.793637468833951));
#21506=CARTESIAN_POINT('',(7.59382715545311,3.06161699786838E-16,-0.793637468833951));
#21507=CARTESIAN_POINT('Origin',(5.09382715545311,0.,-0.793637468833951));
#21508=CARTESIAN_POINT('',(7.59382715545311,3.06161699786838E-16,-3.79363746883395));
#21509=CARTESIAN_POINT('',(7.59382715545311,-3.06161699786838E-16,-0.793637468833951));
#21510=CARTESIAN_POINT('Origin',(5.09382715545311,0.,-3.79363746883395));
#21511=CARTESIAN_POINT('Origin',(9.71262930897012,-1.11022302462516E-15,
-0.793637468833951));
#21512=CARTESIAN_POINT('',(7.40322823221161,-4.,-0.793637468833951));
#21513=CARTESIAN_POINT('',(9.71262930897012,-1.11022302462516E-15,-0.793637468833951));
#21514=CARTESIAN_POINT('',(7.40322823221161,-4.,-0.793637468833951));
#21515=CARTESIAN_POINT('',(7.40322823221161,-4.,-3.79363746883395));
#21516=CARTESIAN_POINT('',(7.40322823221161,-4.,-0.793637468833951));
#21517=CARTESIAN_POINT('',(9.71262930897012,-1.11022302462516E-15,-3.79363746883395));
#21518=CARTESIAN_POINT('',(7.40322823221161,-4.,-3.79363746883395));
#21519=CARTESIAN_POINT('',(9.71262930897012,-1.11022302462516E-15,-0.793637468833951));
#21520=CARTESIAN_POINT('Origin',(7.40322823221161,4.,-0.793637468833951));
#21521=CARTESIAN_POINT('',(7.40322823221161,4.,-0.793637468833951));
#21522=CARTESIAN_POINT('',(9.71262930897012,-1.11022302462516E-15,-0.793637468833951));
#21523=CARTESIAN_POINT('',(7.40322823221161,4.,-3.79363746883395));
#21524=CARTESIAN_POINT('',(9.71262930897012,-1.11022302462516E-15,-3.79363746883395));
#21525=CARTESIAN_POINT('',(7.40322823221161,4.,-0.793637468833951));
#21526=CARTESIAN_POINT('Origin',(2.78442607869461,4.,-0.793637468833951));
#21527=CARTESIAN_POINT('',(2.78442607869461,4.,-0.793637468833951));
#21528=CARTESIAN_POINT('',(7.40322823221161,4.,-0.793637468833951));
#21529=CARTESIAN_POINT('',(2.78442607869461,4.,-3.79363746883395));
#21530=CARTESIAN_POINT('',(7.40322823221161,4.,-3.79363746883395));
#21531=CARTESIAN_POINT('',(2.78442607869461,4.,-0.793637468833951));
#21532=CARTESIAN_POINT('Origin',(0.4750250019361,2.77555756156289E-15,-0.793637468833951));
#21533=CARTESIAN_POINT('',(0.4750250019361,2.77555756156289E-15,-0.793637468833951));
#21534=CARTESIAN_POINT('',(2.78442607869461,4.,-0.793637468833951));
#21535=CARTESIAN_POINT('',(0.4750250019361,2.77555756156289E-15,-3.79363746883395));
#21536=CARTESIAN_POINT('',(2.78442607869461,4.,-3.79363746883395));
#21537=CARTESIAN_POINT('',(0.4750250019361,2.77555756156289E-15,-0.793637468833951));
#21538=CARTESIAN_POINT('Origin',(2.7844260786946,-4.,-0.793637468833951));
#21539=CARTESIAN_POINT('',(2.7844260786946,-4.,-0.793637468833951));
#21540=CARTESIAN_POINT('',(0.4750250019361,2.77555756156289E-15,-0.793637468833951));
#21541=CARTESIAN_POINT('',(2.7844260786946,-4.,-3.79363746883395));
#21542=CARTESIAN_POINT('',(0.4750250019361,2.77555756156289E-15,-3.79363746883395));
#21543=CARTESIAN_POINT('',(2.7844260786946,-4.,-0.793637468833951));
#21544=CARTESIAN_POINT('Origin',(7.40322823221161,-4.,-0.793637468833951));
#21545=CARTESIAN_POINT('',(2.7844260786946,-4.,-0.793637468833951));
#21546=CARTESIAN_POINT('',(2.7844260786946,-4.,-3.79363746883395));
#21547=CARTESIAN_POINT('Origin',(5.09382715545311,5.55111512312578E-16,
-0.793637468833951));
#21548=CARTESIAN_POINT('Origin',(5.09382715545311,5.55111512312578E-16,
-3.79363746883395));
#21549=CARTESIAN_POINT('',(0.,0.,0.));
#21550=CARTESIAN_POINT('Origin',(48.2463073637983,2.63165946910082,69.7993133400953));
#21551=CARTESIAN_POINT('',(68.4030878430531,2.63165946910082,10.8150451223526));
#21552=CARTESIAN_POINT('',(68.4030878430531,3.63165946910082,9.7592393254959));
#21553=CARTESIAN_POINT('Ctrl Pts',(68.4030878430531,2.63165946910082,10.8150451223525));
#21554=CARTESIAN_POINT('Ctrl Pts',(68.4030878430531,2.75292318590158,10.8150451223525));
#21555=CARTESIAN_POINT('Ctrl Pts',(68.4030878430531,2.89541248956616,10.785518210578));
#21556=CARTESIAN_POINT('Ctrl Pts',(68.4030878430531,3.12160772551173,10.6887622121246));
#21557=CARTESIAN_POINT('Ctrl Pts',(68.4030878430531,3.24445614290878,10.6032009112127));
#21558=CARTESIAN_POINT('Ctrl Pts',(68.4030878430531,3.4208720057804,10.4207982530401));
#21559=CARTESIAN_POINT('Ctrl Pts',(68.4030878430531,3.50444108649997,10.2904913846535));
#21560=CARTESIAN_POINT('Ctrl Pts',(68.4030878430531,3.60180286326798,10.0478297006472));
#21561=CARTESIAN_POINT('Ctrl Pts',(68.4030878430531,3.63165946910082,9.89170274555042));
#21562=CARTESIAN_POINT('Ctrl Pts',(68.4030878430531,3.63165946910082,9.75923932549592));
#21563=CARTESIAN_POINT('',(46.2100990071005,3.63165946910082,6.49875929437188));
#21564=CARTESIAN_POINT('Origin',(48.2463073637983,3.63165946910082,69.7993133400953));
#21565=CARTESIAN_POINT('',(46.2422496846979,2.63165946910082,7.49824232770964));
#21566=CARTESIAN_POINT('Origin',(46.2100990071005,2.63165946910082,6.49875929437188));
#21567=CARTESIAN_POINT('Origin',(48.2463073637983,2.63165946910082,69.7993133400953));
#21568=CARTESIAN_POINT('Origin',(47.8424863271981,2.63165946910082,57.2455413903711));
#21569=CARTESIAN_POINT('',(34.7952469924111,3.63165946910083,8.17752607283019));
#21570=CARTESIAN_POINT('',(35.2110476607967,2.63165946910082,9.1019927201825));
#21571=CARTESIAN_POINT('Ctrl Pts',(34.7952469924111,3.63165946910082,8.17752607283017));
#21572=CARTESIAN_POINT('Ctrl Pts',(34.8759799564169,3.63165946910082,8.26626550574801));
#21573=CARTESIAN_POINT('Ctrl Pts',(34.9449983032363,3.61474142049672,8.36195924308515));
#21574=CARTESIAN_POINT('Ctrl Pts',(35.0582831826993,3.53935169168844,8.55821406987691));
#21575=CARTESIAN_POINT('Ctrl Pts',(35.0999567345737,3.48253018537934,8.65414743483824));
#21576=CARTESIAN_POINT('Ctrl Pts',(35.1630116537089,3.32658482415735,8.83595184144993));
#21577=CARTESIAN_POINT('Ctrl Pts',(35.1815579931415,3.22702675024014,8.91709062486395));
#21578=CARTESIAN_POINT('Ctrl Pts',(35.2043257611677,3.00160501814149,9.03961250753693));
#21579=CARTESIAN_POINT('Ctrl Pts',(35.2085733818225,2.87754210657412,9.0797469049714));
#21580=CARTESIAN_POINT('Ctrl Pts',(35.2108030098643,2.71019457520481,9.09967056655112));
#21581=CARTESIAN_POINT('Ctrl Pts',(35.2110476607967,2.67089160721875,9.10199272018252));
#21582=CARTESIAN_POINT('Ctrl Pts',(35.2110476607967,2.63165946910082,9.10199272018252));
#21583=CARTESIAN_POINT('Origin',(47.8424863271981,2.63165946910082,57.2455413903711));
#21584=CARTESIAN_POINT('Origin',(47.8424863271981,3.63165946910082,57.2455413903711));
#21585=CARTESIAN_POINT('Origin',(48.2463073637983,-1.63165946910082,69.7993133400953));
#21586=CARTESIAN_POINT('',(46.2422496846979,-2.63165946910082,7.49824232770964));
#21587=CARTESIAN_POINT('',(46.2422496846979,-1.63165946910082,7.49824232770964));
#21588=CARTESIAN_POINT('',(68.4030878430531,-2.63165946910082,10.8150451223526));
#21589=CARTESIAN_POINT('Origin',(48.2463073637983,-2.63165946910082,69.7993133400953));
#21590=CARTESIAN_POINT('',(68.4030878430531,-1.63165946910082,10.8150451223526));
#21591=CARTESIAN_POINT('Origin',(47.8424863271981,-1.63165946910082,57.2455413903711));
#21592=CARTESIAN_POINT('',(35.2110476607967,-2.63165946910082,9.1019927201825));
#21593=CARTESIAN_POINT('',(35.2110476607967,-1.63165946910082,9.1019927201825));
#21594=CARTESIAN_POINT('Origin',(47.8424863271981,-2.63165946910082,57.2455413903711));
#21595=CARTESIAN_POINT('Origin',(33.5871186320447,-1.63165946910082,9.27665168389945));
#21596=CARTESIAN_POINT('',(33.3825328113569,3.63165946910082,7.65622091215892));
#21597=CARTESIAN_POINT('Origin',(33.5871186320447,3.63165946910082,9.27665168389945));
#21598=CARTESIAN_POINT('',(33.3825328113569,1.63165946910082,7.65622091215892));
#21599=CARTESIAN_POINT('',(33.3825328113569,-1.63165946910082,7.65622091215892));
#21600=CARTESIAN_POINT('',(33.3825328113569,-1.63165946910082,7.65622091215892));
#21601=CARTESIAN_POINT('',(33.3825328113569,-1.63165946910082,7.65622091215892));
#21602=CARTESIAN_POINT('',(33.3825328113569,-3.63165946910082,7.65622091215892));
#21603=CARTESIAN_POINT('',(33.3825328113569,-1.63165946910082,7.65622091215892));
#21604=CARTESIAN_POINT('',(34.7952469924111,-3.63165946910083,8.17752607283019));
#21605=CARTESIAN_POINT('Origin',(33.5871186320447,-3.63165946910082,9.27665168389945));
#21606=CARTESIAN_POINT('Ctrl Pts',(35.2110476607967,-2.63165946910082,9.10199272018252));
#21607=CARTESIAN_POINT('Ctrl Pts',(35.2110476607967,-2.72188359741207,9.10199272018252));
#21608=CARTESIAN_POINT('Ctrl Pts',(35.2098600778781,-2.81173320097753,9.08969048819768));
#21609=CARTESIAN_POINT('Ctrl Pts',(35.2022627780083,-3.02201309856609,9.03140539390586));
#21610=CARTESIAN_POINT('Ctrl Pts',(35.1940414919055,-3.13713858706392,8.97430444925498));
#21611=CARTESIAN_POINT('Ctrl Pts',(35.1597938958569,-3.33127027536278,8.83013309837006));
#21612=CARTESIAN_POINT('Ctrl Pts',(35.1353560110358,-3.41069037668281,8.74720827480345));
#21613=CARTESIAN_POINT('Ctrl Pts',(35.0612832730061,-3.53467292791191,8.56686348527488));
#21614=CARTESIAN_POINT('Ctrl Pts',(35.0133178917238,-3.57786071700438,8.47290631505476));
#21615=CARTESIAN_POINT('Ctrl Pts',(34.9057013358328,-3.62294202580524,8.30910075082814));
#21616=CARTESIAN_POINT('Ctrl Pts',(34.8531835012163,-3.63165946910082,8.24120827501279));
#21617=CARTESIAN_POINT('Ctrl Pts',(34.7952469924111,-3.63165946910082,8.17752607283017));
#21618=CARTESIAN_POINT('Origin',(48.2463073637983,-2.63165946910082,69.7993133400953));
#21619=CARTESIAN_POINT('',(68.4030878430531,-3.63165946910082,9.7592393254959));
#21620=CARTESIAN_POINT('Ctrl Pts',(68.4030878430531,-3.63165946910082,9.75923932549592));
#21621=CARTESIAN_POINT('Ctrl Pts',(68.4030878430531,-3.63165946910082,9.89170274555042));
#21622=CARTESIAN_POINT('Ctrl Pts',(68.4030878430531,-3.60180286326798,10.0478297006472));
#21623=CARTESIAN_POINT('Ctrl Pts',(68.4030878430531,-3.50444108649997,10.2904913846535));
#21624=CARTESIAN_POINT('Ctrl Pts',(68.4030878430531,-3.4208720057804,10.4207982530401));
#21625=CARTESIAN_POINT('Ctrl Pts',(68.4030878430531,-3.24445614290878,10.6032009112127));
#21626=CARTESIAN_POINT('Ctrl Pts',(68.4030878430531,-3.12160772551173,10.6887622121246));
#21627=CARTESIAN_POINT('Ctrl Pts',(68.4030878430531,-2.89541248956616,10.785518210578));
#21628=CARTESIAN_POINT('Ctrl Pts',(68.4030878430531,-2.75292318590158,10.8150451223525));
#21629=CARTESIAN_POINT('Ctrl Pts',(68.4030878430531,-2.63165946910082,10.8150451223525));
#21630=CARTESIAN_POINT('',(46.2100990071005,-3.63165946910082,6.49875929437188));
#21631=CARTESIAN_POINT('Origin',(46.2100990071005,-2.63165946910082,6.49875929437188));
#21632=CARTESIAN_POINT('Origin',(48.2463073637983,-3.63165946910082,69.7993133400953));
#21633=CARTESIAN_POINT('Origin',(47.8424863271981,-2.63165946910082,57.2455413903711));
#21634=CARTESIAN_POINT('Origin',(47.8424863271981,-3.63165946910082,57.2455413903711));
#21635=CARTESIAN_POINT('Origin',(45.1279324444747,-3.63165946910082,5.6095740306375));
#21636=CARTESIAN_POINT('',(25.5295906637922,-3.63165946910082,8.64768604728929));
#21637=CARTESIAN_POINT('',(25.5295906637922,-3.63165946910082,8.64768604728929));
#21638=CARTESIAN_POINT('',(25.3459666144763,-3.63165946910082,3.11371049024365));
#21639=CARTESIAN_POINT('Origin',(24.7143466872546,-3.63165946910082,5.90470262206354));
#21640=CARTESIAN_POINT('',(30.067343367632,-3.63165946910082,1.31927109386626));
#21641=CARTESIAN_POINT('Origin',(25.6749565963595,-3.63165946910082,-3.12914171551276));
#21642=CARTESIAN_POINT('',(34.5886335096989,-3.63165946910082,1.82713536652871));
#21643=CARTESIAN_POINT('Origin',(32.143405418954,-3.63165946910082,3.2164639050219));
#21644=CARTESIAN_POINT('',(68.4030878430531,-3.63165946910082,8.90436665637975));
#21645=CARTESIAN_POINT('Ctrl Pts',(34.5886335096989,-3.63165946910082,1.82713536652871));
#21646=CARTESIAN_POINT('Ctrl Pts',(34.6362092203122,-3.63165946910082,1.88586871178367));
#21647=CARTESIAN_POINT('Ctrl Pts',(34.7347815549813,-3.63165946910082,2.0017194640625));
#21648=CARTESIAN_POINT('Ctrl Pts',(34.8929036972094,-3.63165946910082,2.17064518663626));
#21649=CARTESIAN_POINT('Ctrl Pts',(35.1242660582543,-3.63165946910082,2.38619485268891));
#21650=CARTESIAN_POINT('Ctrl Pts',(35.4484610450702,-3.63165946910082,2.63681988122319));
#21651=CARTESIAN_POINT('Ctrl Pts',(35.8096797219068,-3.63165946910082,2.86110227440431));
#21652=CARTESIAN_POINT('Ctrl Pts',(36.2121827052432,-3.63165946910082,3.0431608239682));
#21653=CARTESIAN_POINT('Ctrl Pts',(36.6605471216616,-3.63165946910082,3.1637619392622));
#21654=CARTESIAN_POINT('Ctrl Pts',(37.1573477919055,-3.63165946910082,3.20674836359645));
#21655=CARTESIAN_POINT('Ctrl Pts',(37.7004983976614,-3.63165946910082,3.16593783342347));
#21656=CARTESIAN_POINT('Ctrl Pts',(38.2821772960432,-3.63165946910082,3.04891646974342));
#21657=CARTESIAN_POINT('Ctrl Pts',(38.8922061650653,-3.63165946910082,2.8717108056677));
#21658=CARTESIAN_POINT('Ctrl Pts',(39.5206820976528,-3.63165946910082,2.655119497821));
#21659=CARTESIAN_POINT('Ctrl Pts',(40.1606960032496,-3.63165946910082,2.42058806459878));
#21660=CARTESIAN_POINT('Ctrl Pts',(40.8115544872912,-3.63165946910082,2.18580974752969));
#21661=CARTESIAN_POINT('Ctrl Pts',(41.4774295553453,-3.63165946910082,1.9643608719398));
#21662=CARTESIAN_POINT('Ctrl Pts',(42.1650261486421,-3.63165946910082,1.76629475930708));
#21663=CARTESIAN_POINT('Ctrl Pts',(42.8815153494359,-3.63165946910082,1.59838107318515));
#21664=CARTESIAN_POINT('Ctrl Pts',(43.6325437023826,-3.63165946910082,1.46450753402197));
#21665=CARTESIAN_POINT('Ctrl Pts',(44.4197406663614,-3.63165946910082,1.36594448830542));
#21666=CARTESIAN_POINT('Ctrl Pts',(45.2407218004933,-3.63165946910082,1.30194849827011));
#21667=CARTESIAN_POINT('Ctrl Pts',(46.0905159507805,-3.63165946910082,1.27053601971253));
#21668=CARTESIAN_POINT('Ctrl Pts',(46.9625249651934,-3.63165946910082,1.26918753879412));
#21669=CARTESIAN_POINT('Ctrl Pts',(47.8497123901009,-3.63165946910082,1.29560818694524));
#21670=CARTESIAN_POINT('Ctrl Pts',(48.745595015671,-3.63165946910082,1.3483918257298));
#21671=CARTESIAN_POINT('Ctrl Pts',(49.6455611586008,-3.63165946910082,1.42790750554685));
#21672=CARTESIAN_POINT('Ctrl Pts',(50.5469014142808,-3.63165946910082,1.53623826938649));
#21673=CARTESIAN_POINT('Ctrl Pts',(51.4480843800216,-3.63165946910082,1.67655609650635));
#21674=CARTESIAN_POINT('Ctrl Pts',(52.348266859532,-3.63165946910082,1.85267033982542));
#21675=CARTESIAN_POINT('Ctrl Pts',(53.2467046577141,-3.63165946910082,2.06850649471347));
#21676=CARTESIAN_POINT('Ctrl Pts',(54.1422176988182,-3.63165946910082,2.32761261079463));
#21677=CARTESIAN_POINT('Ctrl Pts',(55.0326050724517,-3.63165946910082,2.63265678969324));
#21678=CARTESIAN_POINT('Ctrl Pts',(55.9141550877392,-3.63165946910082,2.98491249335729));
#21679=CARTESIAN_POINT('Ctrl Pts',(56.7819405807955,-3.63165946910082,3.3836558364077));
#21680=CARTESIAN_POINT('Ctrl Pts',(57.6300359536437,-3.63165946910082,3.82554246975634));
#21681=CARTESIAN_POINT('Ctrl Pts',(58.4517774296143,-3.63165946910082,4.30403237376386));
#21682=CARTESIAN_POINT('Ctrl Pts',(59.2399671195477,-3.63165946910082,4.80867544303911));
#21683=CARTESIAN_POINT('Ctrl Pts',(59.9871842641414,-3.63165946910082,5.32469977859742));
#21684=CARTESIAN_POINT('Ctrl Pts',(60.6858451039897,-3.63165946910082,5.83183545124052));
#21685=CARTESIAN_POINT('Ctrl Pts',(61.3291075829706,-3.63165946910082,6.30568784052758));
#21686=CARTESIAN_POINT('Ctrl Pts',(61.9129286688635,-3.63165946910082,6.72264590044013));
#21687=CARTESIAN_POINT('Ctrl Pts',(62.4378966914009,-3.63165946910082,7.06401270956655));
#21688=CARTESIAN_POINT('Ctrl Pts',(62.9110626727188,-3.63165946910082,7.32028203996567));
#21689=CARTESIAN_POINT('Ctrl Pts',(63.3480382061253,-3.63165946910082,7.49580221124892));
#21690=CARTESIAN_POINT('Ctrl Pts',(63.7742575841079,-3.63165946910082,7.61203807956635));
#21691=CARTESIAN_POINT('Ctrl Pts',(64.2192519841205,-3.63165946910082,7.69914552267219));
#21692=CARTESIAN_POINT('Ctrl Pts',(64.712086468945,-3.63165946910082,7.78936630198725));
#21693=CARTESIAN_POINT('Ctrl Pts',(65.2754113430736,-3.63165946910082,7.90844857460236));
#21694=CARTESIAN_POINT('Ctrl Pts',(65.9237039528771,-3.63165946910082,8.07283920347654));
#21695=CARTESIAN_POINT('Ctrl Pts',(66.6557369297143,-3.63165946910082,8.28958012503506));
#21696=CARTESIAN_POINT('Ctrl Pts',(67.3150092482541,-3.63165946910082,8.50886642156035));
#21697=CARTESIAN_POINT('Ctrl Pts',(67.8492602326033,-3.63165946910082,8.69890399191606));
#21698=CARTESIAN_POINT('Ctrl Pts',(68.2198703338295,-3.63165946910082,8.83566471550562));
#21699=CARTESIAN_POINT('Ctrl Pts',(68.403087843053,-3.63165946910082,8.90436665637972));
#21700=CARTESIAN_POINT('',(68.4030878430531,-3.63165946910082,8.99271976196806));
#21701=CARTESIAN_POINT('',(34.3381879218756,-3.63165946910082,3.2164639050219));
#21702=CARTESIAN_POINT('Origin',(32.143405418954,-3.63165946910082,3.2164639050219));
#21703=CARTESIAN_POINT('',(26.9156818562223,-3.63165946910082,5.90470262206354));
#21704=CARTESIAN_POINT('Origin',(24.7143466872546,-3.63165946910082,5.90470262206354));
#21705=CARTESIAN_POINT('Origin',(24.7143466872546,-3.63165946910082,5.90470262206354));
#21706=CARTESIAN_POINT('',(26.4156818562223,-3.63165946910082,5.90470262206354));
#21707=CARTESIAN_POINT('Origin',(24.7143466872546,-3.63165946910082,5.90470262206354));
#21708=CARTESIAN_POINT('Origin',(24.7143466872546,-3.38165946910082,5.90470262206354));
#21709=CARTESIAN_POINT('',(26.2085750750357,-4.13165946910082,5.90470262206354));
#21710=CARTESIAN_POINT('Origin',(24.7143466872546,-4.13165946910082,5.90470262206354));
#21711=CARTESIAN_POINT('Origin',(26.2085750750357,-3.38165946910082,5.90470262206354));
#21712=CARTESIAN_POINT('Origin',(24.7143466872546,-4.13165946910082,5.90470262206354));
#21713=CARTESIAN_POINT('Origin',(32.143405418954,-3.63165946910082,3.2164639050219));
#21714=CARTESIAN_POINT('',(33.8381879218756,-3.63165946910082,3.2164639050219));
#21715=CARTESIAN_POINT('Origin',(32.143405418954,-3.63165946910082,3.2164639050219));
#21716=CARTESIAN_POINT('Origin',(32.143405418954,-3.38165946910082,3.2164639050219));
#21717=CARTESIAN_POINT('',(33.6310811406891,-4.13165946910082,3.2164639050219));
#21718=CARTESIAN_POINT('Origin',(32.143405418954,-4.13165946910082,3.2164639050219));
#21719=CARTESIAN_POINT('Origin',(33.6310811406891,-3.38165946910082,3.2164639050219));
#21720=CARTESIAN_POINT('Origin',(32.143405418954,-4.13165946910082,3.2164639050219));
#21721=CARTESIAN_POINT('Origin',(24.7143466872546,3.63165946910082,5.90470262206354));
#21722=CARTESIAN_POINT('',(26.4156818562223,3.63165946910082,5.90470262206354));
#21723=CARTESIAN_POINT('Origin',(24.7143466872546,3.63165946910082,5.90470262206354));
#21724=CARTESIAN_POINT('Origin',(24.7143466872546,3.38165946910082,5.90470262206354));
#21725=CARTESIAN_POINT('',(26.2085750750357,4.13165946910082,5.90470262206354));
#21726=CARTESIAN_POINT('Origin',(24.7143466872546,4.13165946910082,5.90470262206354));
#21727=CARTESIAN_POINT('',(26.9156818562223,3.63165946910082,5.90470262206354));
#21728=CARTESIAN_POINT('Origin',(26.2085750750357,3.38165946910082,5.90470262206354));
#21729=CARTESIAN_POINT('Origin',(24.7143466872546,3.63165946910082,5.90470262206354));
#21730=CARTESIAN_POINT('Origin',(24.7143466872546,4.13165946910082,5.90470262206354));
#21731=CARTESIAN_POINT('Origin',(32.143405418954,3.63165946910082,3.2164639050219));
#21732=CARTESIAN_POINT('',(33.8381879218756,3.63165946910082,3.2164639050219));
#21733=CARTESIAN_POINT('Origin',(32.143405418954,3.63165946910082,3.2164639050219));
#21734=CARTESIAN_POINT('Origin',(32.143405418954,3.38165946910082,3.2164639050219));
#21735=CARTESIAN_POINT('',(33.6310811406891,4.13165946910082,3.2164639050219));
#21736=CARTESIAN_POINT('Origin',(32.143405418954,4.13165946910082,3.2164639050219));
#21737=CARTESIAN_POINT('',(34.3381879218756,3.63165946910082,3.2164639050219));
#21738=CARTESIAN_POINT('Origin',(33.6310811406891,3.38165946910082,3.2164639050219));
#21739=CARTESIAN_POINT('Origin',(32.143405418954,3.63165946910082,3.2164639050219));
#21740=CARTESIAN_POINT('Origin',(32.143405418954,4.13165946910082,3.2164639050219));
#21741=CARTESIAN_POINT('Origin',(32.143405418954,1.63165946910082,3.2164639050219));
#21742=CARTESIAN_POINT('',(33.8381879218756,1.63165946910082,3.2164639050219));
#21743=CARTESIAN_POINT('',(33.8381879218757,1.63165946910082,3.2164639050219));
#21744=CARTESIAN_POINT('Origin',(32.143405418954,1.63165946910082,3.2164639050219));
#21745=CARTESIAN_POINT('Origin',(24.7143466872546,1.63165946910082,5.90470262206354));
#21746=CARTESIAN_POINT('',(26.4156818562223,1.63165946910082,5.90470262206354));
#21747=CARTESIAN_POINT('',(26.4156818562222,1.63165946910082,5.90470262206354));
#21748=CARTESIAN_POINT('Origin',(24.7143466872546,1.63165946910082,5.90470262206354));
#21749=CARTESIAN_POINT('Origin',(33.3825328113569,1.63165946910082,7.65622091215892));
#21750=CARTESIAN_POINT('',(25.5295906637922,1.63165946910082,8.64768604728929));
#21751=CARTESIAN_POINT('',(25.5295906637922,1.63165946910082,8.64768604728929));
#21752=CARTESIAN_POINT('',(25.5295906637922,3.63165946910082,8.64768604728929));
#21753=CARTESIAN_POINT('',(25.5295906637922,3.63165946910082,8.64768604728929));
#21754=CARTESIAN_POINT('',(25.5295906637922,1.63165946910082,8.64768604728929));
#21755=CARTESIAN_POINT('Ctrl Pts',(34.5886335096989,1.63165946910082,1.82713536652871));
#21756=CARTESIAN_POINT('Ctrl Pts',(34.5886335096989,4.03165946910082,1.82713536652871));
#21757=CARTESIAN_POINT('Ctrl Pts',(34.6362092203122,1.63165946910082,1.88586871178367));
#21758=CARTESIAN_POINT('Ctrl Pts',(34.6362092203122,4.03165946910082,1.88586871178367));
#21759=CARTESIAN_POINT('Ctrl Pts',(34.7347815549813,1.63165946910082,2.0017194640625));
#21760=CARTESIAN_POINT('Ctrl Pts',(34.7347815549813,4.03165946910082,2.0017194640625));
#21761=CARTESIAN_POINT('Ctrl Pts',(34.8929036972094,1.63165946910082,2.17064518663626));
#21762=CARTESIAN_POINT('Ctrl Pts',(34.8929036972094,4.03165946910082,2.17064518663626));
#21763=CARTESIAN_POINT('Ctrl Pts',(35.1242660582543,1.63165946910082,2.38619485268891));
#21764=CARTESIAN_POINT('Ctrl Pts',(35.1242660582543,4.03165946910082,2.38619485268891));
#21765=CARTESIAN_POINT('Ctrl Pts',(35.4484610450702,1.63165946910082,2.63681988122319));
#21766=CARTESIAN_POINT('Ctrl Pts',(35.4484610450702,4.03165946910082,2.63681988122319));
#21767=CARTESIAN_POINT('Ctrl Pts',(35.8096797219068,1.63165946910082,2.86110227440431));
#21768=CARTESIAN_POINT('Ctrl Pts',(35.8096797219068,4.03165946910082,2.86110227440431));
#21769=CARTESIAN_POINT('Ctrl Pts',(36.2121827052432,1.63165946910082,3.0431608239682));
#21770=CARTESIAN_POINT('Ctrl Pts',(36.2121827052432,4.03165946910082,3.0431608239682));
#21771=CARTESIAN_POINT('Ctrl Pts',(36.6605471216616,1.63165946910082,3.1637619392622));
#21772=CARTESIAN_POINT('Ctrl Pts',(36.6605471216616,4.03165946910082,3.1637619392622));
#21773=CARTESIAN_POINT('Ctrl Pts',(37.1573477919055,1.63165946910082,3.20674836359645));
#21774=CARTESIAN_POINT('Ctrl Pts',(37.1573477919055,4.03165946910082,3.20674836359645));
#21775=CARTESIAN_POINT('Ctrl Pts',(37.7004983976614,1.63165946910082,3.16593783342347));
#21776=CARTESIAN_POINT('Ctrl Pts',(37.7004983976614,4.03165946910082,3.16593783342347));
#21777=CARTESIAN_POINT('Ctrl Pts',(38.2821772960432,1.63165946910082,3.04891646974342));
#21778=CARTESIAN_POINT('Ctrl Pts',(38.2821772960432,4.03165946910082,3.04891646974342));
#21779=CARTESIAN_POINT('Ctrl Pts',(38.8922061650653,1.63165946910082,2.8717108056677));
#21780=CARTESIAN_POINT('Ctrl Pts',(38.8922061650653,4.03165946910082,2.8717108056677));
#21781=CARTESIAN_POINT('Ctrl Pts',(39.5206820976528,1.63165946910082,2.655119497821));
#21782=CARTESIAN_POINT('Ctrl Pts',(39.5206820976528,4.03165946910082,2.655119497821));
#21783=CARTESIAN_POINT('Ctrl Pts',(40.1606960032496,1.63165946910082,2.42058806459878));
#21784=CARTESIAN_POINT('Ctrl Pts',(40.1606960032496,4.03165946910082,2.42058806459878));
#21785=CARTESIAN_POINT('Ctrl Pts',(40.8115544872912,1.63165946910082,2.18580974752969));
#21786=CARTESIAN_POINT('Ctrl Pts',(40.8115544872912,4.03165946910082,2.18580974752969));
#21787=CARTESIAN_POINT('Ctrl Pts',(41.4774295553453,1.63165946910082,1.9643608719398));
#21788=CARTESIAN_POINT('Ctrl Pts',(41.4774295553453,4.03165946910082,1.9643608719398));
#21789=CARTESIAN_POINT('Ctrl Pts',(42.1650261486421,1.63165946910082,1.76629475930708));
#21790=CARTESIAN_POINT('Ctrl Pts',(42.1650261486421,4.03165946910082,1.76629475930708));
#21791=CARTESIAN_POINT('Ctrl Pts',(42.8815153494359,1.63165946910082,1.59838107318515));
#21792=CARTESIAN_POINT('Ctrl Pts',(42.8815153494359,4.03165946910082,1.59838107318515));
#21793=CARTESIAN_POINT('Ctrl Pts',(43.6325437023826,1.63165946910082,1.46450753402197));
#21794=CARTESIAN_POINT('Ctrl Pts',(43.6325437023826,4.03165946910082,1.46450753402197));
#21795=CARTESIAN_POINT('Ctrl Pts',(44.4197406663614,1.63165946910082,1.36594448830542));
#21796=CARTESIAN_POINT('Ctrl Pts',(44.4197406663614,4.03165946910082,1.36594448830542));
#21797=CARTESIAN_POINT('Ctrl Pts',(45.2407218004933,1.63165946910082,1.30194849827011));
#21798=CARTESIAN_POINT('Ctrl Pts',(45.2407218004933,4.03165946910082,1.30194849827011));
#21799=CARTESIAN_POINT('Ctrl Pts',(46.0905159507805,1.63165946910082,1.27053601971253));
#21800=CARTESIAN_POINT('Ctrl Pts',(46.0905159507805,4.03165946910082,1.27053601971253));
#21801=CARTESIAN_POINT('Ctrl Pts',(46.9625249651934,1.63165946910082,1.26918753879412));
#21802=CARTESIAN_POINT('Ctrl Pts',(46.9625249651934,4.03165946910082,1.26918753879412));
#21803=CARTESIAN_POINT('Ctrl Pts',(47.8497123901009,1.63165946910082,1.29560818694524));
#21804=CARTESIAN_POINT('Ctrl Pts',(47.8497123901009,4.03165946910082,1.29560818694524));
#21805=CARTESIAN_POINT('Ctrl Pts',(48.745595015671,1.63165946910082,1.3483918257298));
#21806=CARTESIAN_POINT('Ctrl Pts',(48.745595015671,4.03165946910082,1.3483918257298));
#21807=CARTESIAN_POINT('Ctrl Pts',(49.6455611586008,1.63165946910082,1.42790750554685));
#21808=CARTESIAN_POINT('Ctrl Pts',(49.6455611586008,4.03165946910082,1.42790750554685));
#21809=CARTESIAN_POINT('Ctrl Pts',(50.5469014142808,1.63165946910082,1.53623826938649));
#21810=CARTESIAN_POINT('Ctrl Pts',(50.5469014142808,4.03165946910082,1.53623826938649));
#21811=CARTESIAN_POINT('Ctrl Pts',(51.4480843800216,1.63165946910082,1.67655609650635));
#21812=CARTESIAN_POINT('Ctrl Pts',(51.4480843800216,4.03165946910082,1.67655609650635));
#21813=CARTESIAN_POINT('Ctrl Pts',(52.348266859532,1.63165946910082,1.85267033982542));
#21814=CARTESIAN_POINT('Ctrl Pts',(52.348266859532,4.03165946910082,1.85267033982542));
#21815=CARTESIAN_POINT('Ctrl Pts',(53.2467046577141,1.63165946910082,2.06850649471347));
#21816=CARTESIAN_POINT('Ctrl Pts',(53.2467046577141,4.03165946910082,2.06850649471347));
#21817=CARTESIAN_POINT('Ctrl Pts',(54.1422176988182,1.63165946910082,2.32761261079463));
#21818=CARTESIAN_POINT('Ctrl Pts',(54.1422176988182,4.03165946910082,2.32761261079463));
#21819=CARTESIAN_POINT('Ctrl Pts',(55.0326050724517,1.63165946910082,2.63265678969324));
#21820=CARTESIAN_POINT('Ctrl Pts',(55.0326050724517,4.03165946910082,2.63265678969324));
#21821=CARTESIAN_POINT('Ctrl Pts',(55.9141550877392,1.63165946910082,2.98491249335729));
#21822=CARTESIAN_POINT('Ctrl Pts',(55.9141550877392,4.03165946910082,2.98491249335729));
#21823=CARTESIAN_POINT('Ctrl Pts',(56.7819405807955,1.63165946910082,3.3836558364077));
#21824=CARTESIAN_POINT('Ctrl Pts',(56.7819405807955,4.03165946910082,3.3836558364077));
#21825=CARTESIAN_POINT('Ctrl Pts',(57.6300359536437,1.63165946910082,3.82554246975634));
#21826=CARTESIAN_POINT('Ctrl Pts',(57.6300359536437,4.03165946910082,3.82554246975634));
#21827=CARTESIAN_POINT('Ctrl Pts',(58.4517774296143,1.63165946910082,4.30403237376386));
#21828=CARTESIAN_POINT('Ctrl Pts',(58.4517774296143,4.03165946910082,4.30403237376386));
#21829=CARTESIAN_POINT('Ctrl Pts',(59.2399671195477,1.63165946910082,4.80867544303911));
#21830=CARTESIAN_POINT('Ctrl Pts',(59.2399671195477,4.03165946910082,4.80867544303911));
#21831=CARTESIAN_POINT('Ctrl Pts',(59.9871842641414,1.63165946910082,5.32469977859742));
#21832=CARTESIAN_POINT('Ctrl Pts',(59.9871842641414,4.03165946910082,5.32469977859742));
#21833=CARTESIAN_POINT('Ctrl Pts',(60.6858451039897,1.63165946910082,5.83183545124052));
#21834=CARTESIAN_POINT('Ctrl Pts',(60.6858451039897,4.03165946910082,5.83183545124052));
#21835=CARTESIAN_POINT('Ctrl Pts',(61.3291075829706,1.63165946910082,6.30568784052758));
#21836=CARTESIAN_POINT('Ctrl Pts',(61.3291075829706,4.03165946910082,6.30568784052758));
#21837=CARTESIAN_POINT('Ctrl Pts',(61.9129286688635,1.63165946910082,6.72264590044013));
#21838=CARTESIAN_POINT('Ctrl Pts',(61.9129286688635,4.03165946910082,6.72264590044013));
#21839=CARTESIAN_POINT('Ctrl Pts',(62.4378966914009,1.63165946910082,7.06401270956655));
#21840=CARTESIAN_POINT('Ctrl Pts',(62.4378966914009,4.03165946910082,7.06401270956655));
#21841=CARTESIAN_POINT('Ctrl Pts',(62.9110626727188,1.63165946910082,7.32028203996567));
#21842=CARTESIAN_POINT('Ctrl Pts',(62.9110626727188,4.03165946910082,7.32028203996567));
#21843=CARTESIAN_POINT('Ctrl Pts',(63.3480382061253,1.63165946910082,7.49580221124892));
#21844=CARTESIAN_POINT('Ctrl Pts',(63.3480382061253,4.03165946910082,7.49580221124892));
#21845=CARTESIAN_POINT('Ctrl Pts',(63.7742575841079,1.63165946910082,7.61203807956635));
#21846=CARTESIAN_POINT('Ctrl Pts',(63.7742575841079,4.03165946910082,7.61203807956635));
#21847=CARTESIAN_POINT('Ctrl Pts',(64.2192519841205,1.63165946910082,7.69914552267219));
#21848=CARTESIAN_POINT('Ctrl Pts',(64.2192519841205,4.03165946910082,7.69914552267219));
#21849=CARTESIAN_POINT('Ctrl Pts',(64.712086468945,1.63165946910082,7.78936630198725));
#21850=CARTESIAN_POINT('Ctrl Pts',(64.712086468945,4.03165946910082,7.78936630198725));
#21851=CARTESIAN_POINT('Ctrl Pts',(65.2754113430736,1.63165946910082,7.90844857460236));
#21852=CARTESIAN_POINT('Ctrl Pts',(65.2754113430736,4.03165946910082,7.90844857460236));
#21853=CARTESIAN_POINT('Ctrl Pts',(65.9237039528771,1.63165946910082,8.07283920347654));
#21854=CARTESIAN_POINT('Ctrl Pts',(65.9237039528771,4.03165946910082,8.07283920347654));
#21855=CARTESIAN_POINT('Ctrl Pts',(66.6557369297143,1.63165946910082,8.28958012503506));
#21856=CARTESIAN_POINT('Ctrl Pts',(66.6557369297143,4.03165946910082,8.28958012503506));
#21857=CARTESIAN_POINT('Ctrl Pts',(67.3150092482541,1.63165946910082,8.50886642156035));
#21858=CARTESIAN_POINT('Ctrl Pts',(67.3150092482541,4.03165946910082,8.50886642156035));
#21859=CARTESIAN_POINT('Ctrl Pts',(67.8492602326033,1.63165946910082,8.69890399191606));
#21860=CARTESIAN_POINT('Ctrl Pts',(67.8492602326033,4.03165946910082,8.69890399191606));
#21861=CARTESIAN_POINT('Ctrl Pts',(68.2198703338295,1.63165946910082,8.83566471550562));
#21862=CARTESIAN_POINT('Ctrl Pts',(68.2198703338295,4.03165946910082,8.83566471550562));
#21863=CARTESIAN_POINT('Ctrl Pts',(68.403087843053,1.63165946910082,8.90436665637972));
#21864=CARTESIAN_POINT('Ctrl Pts',(68.403087843053,4.03165946910082,8.90436665637972));
#21865=CARTESIAN_POINT('',(34.5886335096989,1.63165946910082,1.82713536652871));
#21866=CARTESIAN_POINT('',(68.4030878430531,1.63165946910082,8.90436665637975));
#21867=CARTESIAN_POINT('Ctrl Pts',(34.5886335096989,1.63165946910082,1.82713536652871));
#21868=CARTESIAN_POINT('Ctrl Pts',(34.6362092203122,1.63165946910082,1.88586871178367));
#21869=CARTESIAN_POINT('Ctrl Pts',(34.7347815549813,1.63165946910082,2.0017194640625));
#21870=CARTESIAN_POINT('Ctrl Pts',(34.8929036972094,1.63165946910082,2.17064518663626));
#21871=CARTESIAN_POINT('Ctrl Pts',(35.1242660582543,1.63165946910082,2.38619485268891));
#21872=CARTESIAN_POINT('Ctrl Pts',(35.4484610450702,1.63165946910082,2.63681988122319));
#21873=CARTESIAN_POINT('Ctrl Pts',(35.8096797219068,1.63165946910082,2.86110227440431));
#21874=CARTESIAN_POINT('Ctrl Pts',(36.2121827052432,1.63165946910082,3.0431608239682));
#21875=CARTESIAN_POINT('Ctrl Pts',(36.6605471216616,1.63165946910082,3.1637619392622));
#21876=CARTESIAN_POINT('Ctrl Pts',(37.1573477919055,1.63165946910082,3.20674836359645));
#21877=CARTESIAN_POINT('Ctrl Pts',(37.7004983976614,1.63165946910082,3.16593783342347));
#21878=CARTESIAN_POINT('Ctrl Pts',(38.2821772960432,1.63165946910082,3.04891646974342));
#21879=CARTESIAN_POINT('Ctrl Pts',(38.8922061650653,1.63165946910082,2.8717108056677));
#21880=CARTESIAN_POINT('Ctrl Pts',(39.5206820976528,1.63165946910082,2.655119497821));
#21881=CARTESIAN_POINT('Ctrl Pts',(40.1606960032496,1.63165946910082,2.42058806459878));
#21882=CARTESIAN_POINT('Ctrl Pts',(40.8115544872912,1.63165946910082,2.18580974752969));
#21883=CARTESIAN_POINT('Ctrl Pts',(41.4774295553453,1.63165946910082,1.9643608719398));
#21884=CARTESIAN_POINT('Ctrl Pts',(42.1650261486421,1.63165946910082,1.76629475930708));
#21885=CARTESIAN_POINT('Ctrl Pts',(42.8815153494359,1.63165946910082,1.59838107318515));
#21886=CARTESIAN_POINT('Ctrl Pts',(43.6325437023826,1.63165946910082,1.46450753402197));
#21887=CARTESIAN_POINT('Ctrl Pts',(44.4197406663614,1.63165946910082,1.36594448830542));
#21888=CARTESIAN_POINT('Ctrl Pts',(45.2407218004933,1.63165946910082,1.30194849827011));
#21889=CARTESIAN_POINT('Ctrl Pts',(46.0905159507805,1.63165946910082,1.27053601971253));
#21890=CARTESIAN_POINT('Ctrl Pts',(46.9625249651934,1.63165946910082,1.26918753879412));
#21891=CARTESIAN_POINT('Ctrl Pts',(47.8497123901009,1.63165946910082,1.29560818694524));
#21892=CARTESIAN_POINT('Ctrl Pts',(48.745595015671,1.63165946910082,1.3483918257298));
#21893=CARTESIAN_POINT('Ctrl Pts',(49.6455611586008,1.63165946910082,1.42790750554685));
#21894=CARTESIAN_POINT('Ctrl Pts',(50.5469014142808,1.63165946910082,1.53623826938649));
#21895=CARTESIAN_POINT('Ctrl Pts',(51.4480843800216,1.63165946910082,1.67655609650635));
#21896=CARTESIAN_POINT('Ctrl Pts',(52.348266859532,1.63165946910082,1.85267033982542));
#21897=CARTESIAN_POINT('Ctrl Pts',(53.2467046577141,1.63165946910082,2.06850649471347));
#21898=CARTESIAN_POINT('Ctrl Pts',(54.1422176988182,1.63165946910082,2.32761261079463));
#21899=CARTESIAN_POINT('Ctrl Pts',(55.0326050724517,1.63165946910082,2.63265678969324));
#21900=CARTESIAN_POINT('Ctrl Pts',(55.9141550877392,1.63165946910082,2.98491249335729));
#21901=CARTESIAN_POINT('Ctrl Pts',(56.7819405807955,1.63165946910082,3.3836558364077));
#21902=CARTESIAN_POINT('Ctrl Pts',(57.6300359536437,1.63165946910082,3.82554246975634));
#21903=CARTESIAN_POINT('Ctrl Pts',(58.4517774296143,1.63165946910082,4.30403237376386));
#21904=CARTESIAN_POINT('Ctrl Pts',(59.2399671195477,1.63165946910082,4.80867544303911));
#21905=CARTESIAN_POINT('Ctrl Pts',(59.9871842641414,1.63165946910082,5.32469977859742));
#21906=CARTESIAN_POINT('Ctrl Pts',(60.6858451039897,1.63165946910082,5.83183545124052));
#21907=CARTESIAN_POINT('Ctrl Pts',(61.3291075829706,1.63165946910082,6.30568784052758));
#21908=CARTESIAN_POINT('Ctrl Pts',(61.9129286688635,1.63165946910082,6.72264590044013));
#21909=CARTESIAN_POINT('Ctrl Pts',(62.4378966914009,1.63165946910082,7.06401270956655));
#21910=CARTESIAN_POINT('Ctrl Pts',(62.9110626727188,1.63165946910082,7.32028203996567));
#21911=CARTESIAN_POINT('Ctrl Pts',(63.3480382061253,1.63165946910082,7.49580221124892));
#21912=CARTESIAN_POINT('Ctrl Pts',(63.7742575841079,1.63165946910082,7.61203807956635));
#21913=CARTESIAN_POINT('Ctrl Pts',(64.2192519841205,1.63165946910082,7.69914552267219));
#21914=CARTESIAN_POINT('Ctrl Pts',(64.712086468945,1.63165946910082,7.78936630198725));
#21915=CARTESIAN_POINT('Ctrl Pts',(65.2754113430736,1.63165946910082,7.90844857460236));
#21916=CARTESIAN_POINT('Ctrl Pts',(65.9237039528771,1.63165946910082,8.07283920347654));
#21917=CARTESIAN_POINT('Ctrl Pts',(66.6557369297143,1.63165946910082,8.28958012503506));
#21918=CARTESIAN_POINT('Ctrl Pts',(67.3150092482541,1.63165946910082,8.50886642156036));
#21919=CARTESIAN_POINT('Ctrl Pts',(67.8492602326033,1.63165946910082,8.69890399191607));
#21920=CARTESIAN_POINT('Ctrl Pts',(68.2198703338296,1.63165946910082,8.83566471550565));
#21921=CARTESIAN_POINT('Ctrl Pts',(68.4030878430531,1.63165946910082,8.90436665637975));
#21922=CARTESIAN_POINT('',(34.5886335096989,3.63165946910082,1.82713536652871));
#21923=CARTESIAN_POINT('',(34.5886335096989,1.63165946910082,1.82713536652871));
#21924=CARTESIAN_POINT('',(68.4030878430531,3.63165946910082,8.90436665637975));
#21925=CARTESIAN_POINT('Ctrl Pts',(34.5886335096989,3.63165946910082,1.82713536652871));
#21926=CARTESIAN_POINT('Ctrl Pts',(34.6362092203122,3.63165946910082,1.88586871178367));
#21927=CARTESIAN_POINT('Ctrl Pts',(34.7347815549813,3.63165946910082,2.0017194640625));
#21928=CARTESIAN_POINT('Ctrl Pts',(34.8929036972094,3.63165946910082,2.17064518663626));
#21929=CARTESIAN_POINT('Ctrl Pts',(35.1242660582543,3.63165946910082,2.38619485268891));
#21930=CARTESIAN_POINT('Ctrl Pts',(35.4484610450702,3.63165946910082,2.63681988122319));
#21931=CARTESIAN_POINT('Ctrl Pts',(35.8096797219068,3.63165946910082,2.86110227440431));
#21932=CARTESIAN_POINT('Ctrl Pts',(36.2121827052432,3.63165946910082,3.0431608239682));
#21933=CARTESIAN_POINT('Ctrl Pts',(36.6605471216616,3.63165946910082,3.1637619392622));
#21934=CARTESIAN_POINT('Ctrl Pts',(37.1573477919055,3.63165946910082,3.20674836359645));
#21935=CARTESIAN_POINT('Ctrl Pts',(37.7004983976614,3.63165946910082,3.16593783342347));
#21936=CARTESIAN_POINT('Ctrl Pts',(38.2821772960432,3.63165946910082,3.04891646974342));
#21937=CARTESIAN_POINT('Ctrl Pts',(38.8922061650653,3.63165946910082,2.8717108056677));
#21938=CARTESIAN_POINT('Ctrl Pts',(39.5206820976528,3.63165946910082,2.655119497821));
#21939=CARTESIAN_POINT('Ctrl Pts',(40.1606960032496,3.63165946910082,2.42058806459878));
#21940=CARTESIAN_POINT('Ctrl Pts',(40.8115544872912,3.63165946910082,2.18580974752969));
#21941=CARTESIAN_POINT('Ctrl Pts',(41.4774295553453,3.63165946910082,1.9643608719398));
#21942=CARTESIAN_POINT('Ctrl Pts',(42.1650261486421,3.63165946910082,1.76629475930708));
#21943=CARTESIAN_POINT('Ctrl Pts',(42.8815153494359,3.63165946910082,1.59838107318515));
#21944=CARTESIAN_POINT('Ctrl Pts',(43.6325437023826,3.63165946910082,1.46450753402197));
#21945=CARTESIAN_POINT('Ctrl Pts',(44.4197406663614,3.63165946910082,1.36594448830542));
#21946=CARTESIAN_POINT('Ctrl Pts',(45.2407218004933,3.63165946910082,1.30194849827011));
#21947=CARTESIAN_POINT('Ctrl Pts',(46.0905159507805,3.63165946910082,1.27053601971253));
#21948=CARTESIAN_POINT('Ctrl Pts',(46.9625249651934,3.63165946910082,1.26918753879412));
#21949=CARTESIAN_POINT('Ctrl Pts',(47.8497123901009,3.63165946910082,1.29560818694524));
#21950=CARTESIAN_POINT('Ctrl Pts',(48.745595015671,3.63165946910082,1.3483918257298));
#21951=CARTESIAN_POINT('Ctrl Pts',(49.6455611586008,3.63165946910082,1.42790750554685));
#21952=CARTESIAN_POINT('Ctrl Pts',(50.5469014142808,3.63165946910082,1.53623826938649));
#21953=CARTESIAN_POINT('Ctrl Pts',(51.4480843800216,3.63165946910082,1.67655609650635));
#21954=CARTESIAN_POINT('Ctrl Pts',(52.348266859532,3.63165946910082,1.85267033982542));
#21955=CARTESIAN_POINT('Ctrl Pts',(53.2467046577141,3.63165946910082,2.06850649471347));
#21956=CARTESIAN_POINT('Ctrl Pts',(54.1422176988182,3.63165946910082,2.32761261079463));
#21957=CARTESIAN_POINT('Ctrl Pts',(55.0326050724517,3.63165946910082,2.63265678969324));
#21958=CARTESIAN_POINT('Ctrl Pts',(55.9141550877392,3.63165946910082,2.98491249335729));
#21959=CARTESIAN_POINT('Ctrl Pts',(56.7819405807955,3.63165946910082,3.3836558364077));
#21960=CARTESIAN_POINT('Ctrl Pts',(57.6300359536437,3.63165946910082,3.82554246975634));
#21961=CARTESIAN_POINT('Ctrl Pts',(58.4517774296143,3.63165946910082,4.30403237376386));
#21962=CARTESIAN_POINT('Ctrl Pts',(59.2399671195477,3.63165946910082,4.80867544303911));
#21963=CARTESIAN_POINT('Ctrl Pts',(59.9871842641414,3.63165946910082,5.32469977859742));
#21964=CARTESIAN_POINT('Ctrl Pts',(60.6858451039897,3.63165946910082,5.83183545124052));
#21965=CARTESIAN_POINT('Ctrl Pts',(61.3291075829706,3.63165946910082,6.30568784052758));
#21966=CARTESIAN_POINT('Ctrl Pts',(61.9129286688635,3.63165946910082,6.72264590044013));
#21967=CARTESIAN_POINT('Ctrl Pts',(62.4378966914009,3.63165946910082,7.06401270956655));
#21968=CARTESIAN_POINT('Ctrl Pts',(62.9110626727188,3.63165946910082,7.32028203996567));
#21969=CARTESIAN_POINT('Ctrl Pts',(63.3480382061253,3.63165946910082,7.49580221124892));
#21970=CARTESIAN_POINT('Ctrl Pts',(63.7742575841079,3.63165946910082,7.61203807956635));
#21971=CARTESIAN_POINT('Ctrl Pts',(64.2192519841205,3.63165946910082,7.69914552267219));
#21972=CARTESIAN_POINT('Ctrl Pts',(64.712086468945,3.63165946910082,7.78936630198725));
#21973=CARTESIAN_POINT('Ctrl Pts',(65.2754113430736,3.63165946910082,7.90844857460236));
#21974=CARTESIAN_POINT('Ctrl Pts',(65.9237039528771,3.63165946910082,8.07283920347654));
#21975=CARTESIAN_POINT('Ctrl Pts',(66.6557369297143,3.63165946910082,8.28958012503506));
#21976=CARTESIAN_POINT('Ctrl Pts',(67.3150092482541,3.63165946910082,8.50886642156035));
#21977=CARTESIAN_POINT('Ctrl Pts',(67.8492602326033,3.63165946910082,8.69890399191606));
#21978=CARTESIAN_POINT('Ctrl Pts',(68.2198703338295,3.63165946910082,8.83566471550562));
#21979=CARTESIAN_POINT('Ctrl Pts',(68.403087843053,3.63165946910082,8.90436665637972));
#21980=CARTESIAN_POINT('',(68.4030878430531,1.63165946910082,8.90436665637975));
#21981=CARTESIAN_POINT('Origin',(32.143405418954,1.63165946910082,3.2164639050219));
#21982=CARTESIAN_POINT('',(30.067343367632,1.63165946910082,1.31927109386626));
#21983=CARTESIAN_POINT('Origin',(32.143405418954,1.63165946910082,3.2164639050219));
#21984=CARTESIAN_POINT('',(30.067343367632,3.63165946910082,1.31927109386626));
#21985=CARTESIAN_POINT('',(30.067343367632,1.63165946910082,1.31927109386626));
#21986=CARTESIAN_POINT('Origin',(32.143405418954,3.63165946910082,3.2164639050219));
#21987=CARTESIAN_POINT('Origin',(25.6749565963595,1.63165946910082,-3.12914171551276));
#21988=CARTESIAN_POINT('',(25.3459666144763,1.63165946910082,3.11371049024365));
#21989=CARTESIAN_POINT('Origin',(25.6749565963595,1.63165946910082,-3.12914171551276));
#21990=CARTESIAN_POINT('',(25.3459666144763,3.63165946910082,3.11371049024365));
#21991=CARTESIAN_POINT('',(25.3459666144763,1.63165946910082,3.11371049024365));
#21992=CARTESIAN_POINT('Origin',(25.6749565963595,3.63165946910082,-3.12914171551276));
#21993=CARTESIAN_POINT('Origin',(24.7143466872546,1.63165946910082,5.90470262206354));
#21994=CARTESIAN_POINT('Origin',(24.7143466872546,1.63165946910082,5.90470262206354));
#21995=CARTESIAN_POINT('Origin',(24.7143466872546,3.63165946910082,5.90470262206354));
#21996=CARTESIAN_POINT('Origin',(45.1279324444747,3.63165946910082,5.6095740306375));
#21997=CARTESIAN_POINT('',(68.4030878430531,3.63165946910082,8.99271976196806));
#21998=CARTESIAN_POINT('Origin',(45.1279324444747,1.63165946910082,5.6095740306375));
#21999=CARTESIAN_POINT('',(34.7727361660163,1.63165946910082,7.43140939717669));
#22000=CARTESIAN_POINT('',(39.9619395364675,1.63165946910082,6.59225686071356));
#22001=CARTESIAN_POINT('',(68.4030878430531,1.63165946910082,8.99271976196808));
#22002=CARTESIAN_POINT('',(68.4030878430531,1.63165946910082,8.99271976196806));
#22003=CARTESIAN_POINT('',(46.1867214006044,1.63165946910082,5.77200879332694));
#22004=CARTESIAN_POINT('Origin',(48.2463073637983,1.63165946910082,69.7993133400953));
#22005=CARTESIAN_POINT('Origin',(47.8424863271981,1.63165946910082,57.2455413903711));
#22006=CARTESIAN_POINT('Origin',(34.7727361660163,-1.63165946910082,7.43140939717669));
#22007=CARTESIAN_POINT('',(34.7727361660163,-1.63165946910082,7.43140939717669));
#22008=CARTESIAN_POINT('',(34.7727361660163,-1.63165946910082,7.43140939717669));
#22009=CARTESIAN_POINT('',(39.9619395364675,-1.63165946910082,6.59225686071356));
#22010=CARTESIAN_POINT('Origin',(47.8424863271981,-1.63165946910082,57.2455413903711));
#22011=CARTESIAN_POINT('',(46.1867214006044,-1.63165946910082,5.77200879332694));
#22012=CARTESIAN_POINT('',(46.1867214006044,-1.63165946910082,5.77200879332694));
#22013=CARTESIAN_POINT('Origin',(47.8424863271981,-1.63165946910082,57.2455413903711));
#22014=CARTESIAN_POINT('Origin',(48.2463073637983,-1.63165946910082,69.7993133400953));
#22015=CARTESIAN_POINT('',(68.4030878430531,-1.63165946910082,8.99271976196806));
#22016=CARTESIAN_POINT('',(68.4030878430531,-1.63165946910082,8.99271976196806));
#22017=CARTESIAN_POINT('Origin',(48.2463073637983,-1.63165946910082,69.7993133400953));
#22018=CARTESIAN_POINT('Origin',(45.1279324444747,-1.63165946910082,5.6095740306375));
#22019=CARTESIAN_POINT('',(68.4030878430531,-1.63165946910082,8.90436665637975));
#22020=CARTESIAN_POINT('',(68.4030878430531,-1.63165946910082,8.99271976196806));
#22021=CARTESIAN_POINT('',(34.5886335096989,-1.63165946910082,1.82713536652871));
#22022=CARTESIAN_POINT('Ctrl Pts',(34.5886335096989,-1.63165946910082,1.82713536652871));
#22023=CARTESIAN_POINT('Ctrl Pts',(34.6362092203122,-1.63165946910082,1.88586871178367));
#22024=CARTESIAN_POINT('Ctrl Pts',(34.7347815549813,-1.63165946910082,2.0017194640625));
#22025=CARTESIAN_POINT('Ctrl Pts',(34.8929036972094,-1.63165946910082,2.17064518663626));
#22026=CARTESIAN_POINT('Ctrl Pts',(35.1242660582543,-1.63165946910082,2.38619485268891));
#22027=CARTESIAN_POINT('Ctrl Pts',(35.4484610450702,-1.63165946910082,2.63681988122319));
#22028=CARTESIAN_POINT('Ctrl Pts',(35.8096797219068,-1.63165946910082,2.86110227440431));
#22029=CARTESIAN_POINT('Ctrl Pts',(36.2121827052432,-1.63165946910082,3.0431608239682));
#22030=CARTESIAN_POINT('Ctrl Pts',(36.6605471216616,-1.63165946910082,3.1637619392622));
#22031=CARTESIAN_POINT('Ctrl Pts',(37.1573477919055,-1.63165946910082,3.20674836359645));
#22032=CARTESIAN_POINT('Ctrl Pts',(37.7004983976614,-1.63165946910082,3.16593783342347));
#22033=CARTESIAN_POINT('Ctrl Pts',(38.2821772960432,-1.63165946910082,3.04891646974342));
#22034=CARTESIAN_POINT('Ctrl Pts',(38.8922061650653,-1.63165946910082,2.8717108056677));
#22035=CARTESIAN_POINT('Ctrl Pts',(39.5206820976528,-1.63165946910082,2.655119497821));
#22036=CARTESIAN_POINT('Ctrl Pts',(40.1606960032496,-1.63165946910082,2.42058806459878));
#22037=CARTESIAN_POINT('Ctrl Pts',(40.8115544872912,-1.63165946910082,2.18580974752969));
#22038=CARTESIAN_POINT('Ctrl Pts',(41.4774295553453,-1.63165946910082,1.9643608719398));
#22039=CARTESIAN_POINT('Ctrl Pts',(42.1650261486421,-1.63165946910082,1.76629475930708));
#22040=CARTESIAN_POINT('Ctrl Pts',(42.8815153494359,-1.63165946910082,1.59838107318515));
#22041=CARTESIAN_POINT('Ctrl Pts',(43.6325437023826,-1.63165946910082,1.46450753402197));
#22042=CARTESIAN_POINT('Ctrl Pts',(44.4197406663614,-1.63165946910082,1.36594448830542));
#22043=CARTESIAN_POINT('Ctrl Pts',(45.2407218004933,-1.63165946910082,1.30194849827011));
#22044=CARTESIAN_POINT('Ctrl Pts',(46.0905159507805,-1.63165946910082,1.27053601971253));
#22045=CARTESIAN_POINT('Ctrl Pts',(46.9625249651934,-1.63165946910082,1.26918753879412));
#22046=CARTESIAN_POINT('Ctrl Pts',(47.8497123901009,-1.63165946910082,1.29560818694524));
#22047=CARTESIAN_POINT('Ctrl Pts',(48.745595015671,-1.63165946910082,1.3483918257298));
#22048=CARTESIAN_POINT('Ctrl Pts',(49.6455611586008,-1.63165946910082,1.42790750554685));
#22049=CARTESIAN_POINT('Ctrl Pts',(50.5469014142808,-1.63165946910082,1.53623826938649));
#22050=CARTESIAN_POINT('Ctrl Pts',(51.4480843800216,-1.63165946910082,1.67655609650635));
#22051=CARTESIAN_POINT('Ctrl Pts',(52.348266859532,-1.63165946910082,1.85267033982542));
#22052=CARTESIAN_POINT('Ctrl Pts',(53.2467046577141,-1.63165946910082,2.06850649471347));
#22053=CARTESIAN_POINT('Ctrl Pts',(54.1422176988182,-1.63165946910082,2.32761261079463));
#22054=CARTESIAN_POINT('Ctrl Pts',(55.0326050724517,-1.63165946910082,2.63265678969324));
#22055=CARTESIAN_POINT('Ctrl Pts',(55.9141550877392,-1.63165946910082,2.98491249335729));
#22056=CARTESIAN_POINT('Ctrl Pts',(56.7819405807955,-1.63165946910082,3.3836558364077));
#22057=CARTESIAN_POINT('Ctrl Pts',(57.6300359536437,-1.63165946910082,3.82554246975634));
#22058=CARTESIAN_POINT('Ctrl Pts',(58.4517774296143,-1.63165946910082,4.30403237376386));
#22059=CARTESIAN_POINT('Ctrl Pts',(59.2399671195477,-1.63165946910082,4.80867544303911));
#22060=CARTESIAN_POINT('Ctrl Pts',(59.9871842641414,-1.63165946910082,5.32469977859742));
#22061=CARTESIAN_POINT('Ctrl Pts',(60.6858451039897,-1.63165946910082,5.83183545124052));
#22062=CARTESIAN_POINT('Ctrl Pts',(61.3291075829706,-1.63165946910082,6.30568784052758));
#22063=CARTESIAN_POINT('Ctrl Pts',(61.9129286688635,-1.63165946910082,6.72264590044013));
#22064=CARTESIAN_POINT('Ctrl Pts',(62.4378966914009,-1.63165946910082,7.06401270956655));
#22065=CARTESIAN_POINT('Ctrl Pts',(62.9110626727188,-1.63165946910082,7.32028203996567));
#22066=CARTESIAN_POINT('Ctrl Pts',(63.3480382061253,-1.63165946910082,7.49580221124892));
#22067=CARTESIAN_POINT('Ctrl Pts',(63.7742575841079,-1.63165946910082,7.61203807956635));
#22068=CARTESIAN_POINT('Ctrl Pts',(64.2192519841205,-1.63165946910082,7.69914552267219));
#22069=CARTESIAN_POINT('Ctrl Pts',(64.712086468945,-1.63165946910082,7.78936630198725));
#22070=CARTESIAN_POINT('Ctrl Pts',(65.2754113430736,-1.63165946910082,7.90844857460236));
#22071=CARTESIAN_POINT('Ctrl Pts',(65.9237039528771,-1.63165946910082,8.07283920347654));
#22072=CARTESIAN_POINT('Ctrl Pts',(66.6557369297143,-1.63165946910082,8.28958012503506));
#22073=CARTESIAN_POINT('Ctrl Pts',(67.3150092482541,-1.63165946910082,8.50886642156036));
#22074=CARTESIAN_POINT('Ctrl Pts',(67.8492602326033,-1.63165946910082,8.69890399191607));
#22075=CARTESIAN_POINT('Ctrl Pts',(68.2198703338296,-1.63165946910082,8.83566471550565));
#22076=CARTESIAN_POINT('Ctrl Pts',(68.4030878430531,-1.63165946910082,8.90436665637975));
#22077=CARTESIAN_POINT('',(30.067343367632,-1.63165946910082,1.31927109386626));
#22078=CARTESIAN_POINT('Origin',(32.143405418954,-1.63165946910082,3.2164639050219));
#22079=CARTESIAN_POINT('',(25.3459666144763,-1.63165946910082,3.11371049024365));
#22080=CARTESIAN_POINT('Origin',(25.6749565963595,-1.63165946910082,-3.12914171551276));
#22081=CARTESIAN_POINT('',(25.5295906637922,-1.63165946910082,8.64768604728929));
#22082=CARTESIAN_POINT('Origin',(24.7143466872546,-1.63165946910082,5.90470262206354));
#22083=CARTESIAN_POINT('',(25.5295906637922,-1.63165946910082,8.64768604728929));
#22084=CARTESIAN_POINT('',(33.8381879218756,-1.63165946910082,3.2164639050219));
#22085=CARTESIAN_POINT('Origin',(32.143405418954,-1.63165946910082,3.2164639050219));
#22086=CARTESIAN_POINT('',(26.4156818562223,-1.63165946910082,5.90470262206354));
#22087=CARTESIAN_POINT('Origin',(24.7143466872546,-1.63165946910082,5.90470262206354));
#22088=CARTESIAN_POINT('Origin',(32.143405418954,-1.63165946910082,3.2164639050219));
#22089=CARTESIAN_POINT('',(33.8381879218757,-1.63165946910082,3.2164639050219));
#22090=CARTESIAN_POINT('Origin',(24.7143466872546,-1.63165946910082,5.90470262206354));
#22091=CARTESIAN_POINT('',(26.4156818562222,-1.63165946910082,5.90470262206354));
#22092=CARTESIAN_POINT('Origin',(33.3825328113569,-1.63165946910082,7.65622091215892));
#22093=CARTESIAN_POINT('',(25.5295906637922,-1.63165946910082,8.64768604728929));
#22094=CARTESIAN_POINT('Origin',(68.4030878430531,-1.63165946910082,8.90436665637975));
#22095=CARTESIAN_POINT('',(68.4030878430531,-1.63165946910082,8.90436665637975));
#22096=CARTESIAN_POINT('Ctrl Pts',(34.5886335096989,-1.63165946910082,1.82713536652871));
#22097=CARTESIAN_POINT('Ctrl Pts',(34.5886335096989,-4.03165946910082,1.82713536652871));
#22098=CARTESIAN_POINT('Ctrl Pts',(34.6362092203122,-1.63165946910082,1.88586871178367));
#22099=CARTESIAN_POINT('Ctrl Pts',(34.6362092203122,-4.03165946910082,1.88586871178367));
#22100=CARTESIAN_POINT('Ctrl Pts',(34.7347815549813,-1.63165946910082,2.0017194640625));
#22101=CARTESIAN_POINT('Ctrl Pts',(34.7347815549813,-4.03165946910082,2.0017194640625));
#22102=CARTESIAN_POINT('Ctrl Pts',(34.8929036972094,-1.63165946910082,2.17064518663626));
#22103=CARTESIAN_POINT('Ctrl Pts',(34.8929036972094,-4.03165946910082,2.17064518663626));
#22104=CARTESIAN_POINT('Ctrl Pts',(35.1242660582543,-1.63165946910082,2.38619485268891));
#22105=CARTESIAN_POINT('Ctrl Pts',(35.1242660582543,-4.03165946910082,2.38619485268891));
#22106=CARTESIAN_POINT('Ctrl Pts',(35.4484610450702,-1.63165946910082,2.63681988122319));
#22107=CARTESIAN_POINT('Ctrl Pts',(35.4484610450702,-4.03165946910082,2.63681988122319));
#22108=CARTESIAN_POINT('Ctrl Pts',(35.8096797219068,-1.63165946910082,2.86110227440431));
#22109=CARTESIAN_POINT('Ctrl Pts',(35.8096797219068,-4.03165946910082,2.86110227440431));
#22110=CARTESIAN_POINT('Ctrl Pts',(36.2121827052432,-1.63165946910082,3.0431608239682));
#22111=CARTESIAN_POINT('Ctrl Pts',(36.2121827052432,-4.03165946910082,3.0431608239682));
#22112=CARTESIAN_POINT('Ctrl Pts',(36.6605471216616,-1.63165946910082,3.1637619392622));
#22113=CARTESIAN_POINT('Ctrl Pts',(36.6605471216616,-4.03165946910082,3.1637619392622));
#22114=CARTESIAN_POINT('Ctrl Pts',(37.1573477919055,-1.63165946910082,3.20674836359645));
#22115=CARTESIAN_POINT('Ctrl Pts',(37.1573477919055,-4.03165946910082,3.20674836359645));
#22116=CARTESIAN_POINT('Ctrl Pts',(37.7004983976614,-1.63165946910082,3.16593783342347));
#22117=CARTESIAN_POINT('Ctrl Pts',(37.7004983976614,-4.03165946910082,3.16593783342347));
#22118=CARTESIAN_POINT('Ctrl Pts',(38.2821772960432,-1.63165946910082,3.04891646974342));
#22119=CARTESIAN_POINT('Ctrl Pts',(38.2821772960432,-4.03165946910082,3.04891646974342));
#22120=CARTESIAN_POINT('Ctrl Pts',(38.8922061650653,-1.63165946910082,2.8717108056677));
#22121=CARTESIAN_POINT('Ctrl Pts',(38.8922061650653,-4.03165946910082,2.8717108056677));
#22122=CARTESIAN_POINT('Ctrl Pts',(39.5206820976528,-1.63165946910082,2.655119497821));
#22123=CARTESIAN_POINT('Ctrl Pts',(39.5206820976528,-4.03165946910082,2.655119497821));
#22124=CARTESIAN_POINT('Ctrl Pts',(40.1606960032496,-1.63165946910082,2.42058806459878));
#22125=CARTESIAN_POINT('Ctrl Pts',(40.1606960032496,-4.03165946910082,2.42058806459878));
#22126=CARTESIAN_POINT('Ctrl Pts',(40.8115544872912,-1.63165946910082,2.18580974752969));
#22127=CARTESIAN_POINT('Ctrl Pts',(40.8115544872912,-4.03165946910082,2.18580974752969));
#22128=CARTESIAN_POINT('Ctrl Pts',(41.4774295553453,-1.63165946910082,1.9643608719398));
#22129=CARTESIAN_POINT('Ctrl Pts',(41.4774295553453,-4.03165946910082,1.9643608719398));
#22130=CARTESIAN_POINT('Ctrl Pts',(42.1650261486421,-1.63165946910082,1.76629475930708));
#22131=CARTESIAN_POINT('Ctrl Pts',(42.1650261486421,-4.03165946910082,1.76629475930708));
#22132=CARTESIAN_POINT('Ctrl Pts',(42.8815153494359,-1.63165946910082,1.59838107318515));
#22133=CARTESIAN_POINT('Ctrl Pts',(42.8815153494359,-4.03165946910082,1.59838107318515));
#22134=CARTESIAN_POINT('Ctrl Pts',(43.6325437023826,-1.63165946910082,1.46450753402197));
#22135=CARTESIAN_POINT('Ctrl Pts',(43.6325437023826,-4.03165946910082,1.46450753402197));
#22136=CARTESIAN_POINT('Ctrl Pts',(44.4197406663614,-1.63165946910082,1.36594448830542));
#22137=CARTESIAN_POINT('Ctrl Pts',(44.4197406663614,-4.03165946910082,1.36594448830542));
#22138=CARTESIAN_POINT('Ctrl Pts',(45.2407218004933,-1.63165946910082,1.30194849827011));
#22139=CARTESIAN_POINT('Ctrl Pts',(45.2407218004933,-4.03165946910082,1.30194849827011));
#22140=CARTESIAN_POINT('Ctrl Pts',(46.0905159507805,-1.63165946910082,1.27053601971253));
#22141=CARTESIAN_POINT('Ctrl Pts',(46.0905159507805,-4.03165946910082,1.27053601971253));
#22142=CARTESIAN_POINT('Ctrl Pts',(46.9625249651934,-1.63165946910082,1.26918753879412));
#22143=CARTESIAN_POINT('Ctrl Pts',(46.9625249651934,-4.03165946910082,1.26918753879412));
#22144=CARTESIAN_POINT('Ctrl Pts',(47.8497123901009,-1.63165946910082,1.29560818694524));
#22145=CARTESIAN_POINT('Ctrl Pts',(47.8497123901009,-4.03165946910082,1.29560818694524));
#22146=CARTESIAN_POINT('Ctrl Pts',(48.745595015671,-1.63165946910082,1.3483918257298));
#22147=CARTESIAN_POINT('Ctrl Pts',(48.745595015671,-4.03165946910082,1.3483918257298));
#22148=CARTESIAN_POINT('Ctrl Pts',(49.6455611586008,-1.63165946910082,1.42790750554685));
#22149=CARTESIAN_POINT('Ctrl Pts',(49.6455611586008,-4.03165946910082,1.42790750554685));
#22150=CARTESIAN_POINT('Ctrl Pts',(50.5469014142808,-1.63165946910082,1.53623826938649));
#22151=CARTESIAN_POINT('Ctrl Pts',(50.5469014142808,-4.03165946910082,1.53623826938649));
#22152=CARTESIAN_POINT('Ctrl Pts',(51.4480843800216,-1.63165946910082,1.67655609650635));
#22153=CARTESIAN_POINT('Ctrl Pts',(51.4480843800216,-4.03165946910082,1.67655609650635));
#22154=CARTESIAN_POINT('Ctrl Pts',(52.348266859532,-1.63165946910082,1.85267033982542));
#22155=CARTESIAN_POINT('Ctrl Pts',(52.348266859532,-4.03165946910082,1.85267033982542));
#22156=CARTESIAN_POINT('Ctrl Pts',(53.2467046577141,-1.63165946910082,2.06850649471347));
#22157=CARTESIAN_POINT('Ctrl Pts',(53.2467046577141,-4.03165946910082,2.06850649471347));
#22158=CARTESIAN_POINT('Ctrl Pts',(54.1422176988182,-1.63165946910082,2.32761261079463));
#22159=CARTESIAN_POINT('Ctrl Pts',(54.1422176988182,-4.03165946910082,2.32761261079463));
#22160=CARTESIAN_POINT('Ctrl Pts',(55.0326050724517,-1.63165946910082,2.63265678969324));
#22161=CARTESIAN_POINT('Ctrl Pts',(55.0326050724517,-4.03165946910082,2.63265678969324));
#22162=CARTESIAN_POINT('Ctrl Pts',(55.9141550877392,-1.63165946910082,2.98491249335729));
#22163=CARTESIAN_POINT('Ctrl Pts',(55.9141550877392,-4.03165946910082,2.98491249335729));
#22164=CARTESIAN_POINT('Ctrl Pts',(56.7819405807955,-1.63165946910082,3.3836558364077));
#22165=CARTESIAN_POINT('Ctrl Pts',(56.7819405807955,-4.03165946910082,3.3836558364077));
#22166=CARTESIAN_POINT('Ctrl Pts',(57.6300359536437,-1.63165946910082,3.82554246975634));
#22167=CARTESIAN_POINT('Ctrl Pts',(57.6300359536437,-4.03165946910082,3.82554246975634));
#22168=CARTESIAN_POINT('Ctrl Pts',(58.4517774296143,-1.63165946910082,4.30403237376386));
#22169=CARTESIAN_POINT('Ctrl Pts',(58.4517774296143,-4.03165946910082,4.30403237376386));
#22170=CARTESIAN_POINT('Ctrl Pts',(59.2399671195477,-1.63165946910082,4.80867544303911));
#22171=CARTESIAN_POINT('Ctrl Pts',(59.2399671195477,-4.03165946910082,4.80867544303911));
#22172=CARTESIAN_POINT('Ctrl Pts',(59.9871842641414,-1.63165946910082,5.32469977859742));
#22173=CARTESIAN_POINT('Ctrl Pts',(59.9871842641414,-4.03165946910082,5.32469977859742));
#22174=CARTESIAN_POINT('Ctrl Pts',(60.6858451039897,-1.63165946910082,5.83183545124052));
#22175=CARTESIAN_POINT('Ctrl Pts',(60.6858451039897,-4.03165946910082,5.83183545124052));
#22176=CARTESIAN_POINT('Ctrl Pts',(61.3291075829706,-1.63165946910082,6.30568784052758));
#22177=CARTESIAN_POINT('Ctrl Pts',(61.3291075829706,-4.03165946910082,6.30568784052758));
#22178=CARTESIAN_POINT('Ctrl Pts',(61.9129286688635,-1.63165946910082,6.72264590044013));
#22179=CARTESIAN_POINT('Ctrl Pts',(61.9129286688635,-4.03165946910082,6.72264590044013));
#22180=CARTESIAN_POINT('Ctrl Pts',(62.4378966914009,-1.63165946910082,7.06401270956655));
#22181=CARTESIAN_POINT('Ctrl Pts',(62.4378966914009,-4.03165946910082,7.06401270956655));
#22182=CARTESIAN_POINT('Ctrl Pts',(62.9110626727188,-1.63165946910082,7.32028203996567));
#22183=CARTESIAN_POINT('Ctrl Pts',(62.9110626727188,-4.03165946910082,7.32028203996567));
#22184=CARTESIAN_POINT('Ctrl Pts',(63.3480382061253,-1.63165946910082,7.49580221124892));
#22185=CARTESIAN_POINT('Ctrl Pts',(63.3480382061253,-4.03165946910082,7.49580221124892));
#22186=CARTESIAN_POINT('Ctrl Pts',(63.7742575841079,-1.63165946910082,7.61203807956635));
#22187=CARTESIAN_POINT('Ctrl Pts',(63.7742575841079,-4.03165946910082,7.61203807956635));
#22188=CARTESIAN_POINT('Ctrl Pts',(64.2192519841205,-1.63165946910082,7.69914552267219));
#22189=CARTESIAN_POINT('Ctrl Pts',(64.2192519841205,-4.03165946910082,7.69914552267219));
#22190=CARTESIAN_POINT('Ctrl Pts',(64.712086468945,-1.63165946910082,7.78936630198725));
#22191=CARTESIAN_POINT('Ctrl Pts',(64.712086468945,-4.03165946910082,7.78936630198725));
#22192=CARTESIAN_POINT('Ctrl Pts',(65.2754113430736,-1.63165946910082,7.90844857460236));
#22193=CARTESIAN_POINT('Ctrl Pts',(65.2754113430736,-4.03165946910082,7.90844857460236));
#22194=CARTESIAN_POINT('Ctrl Pts',(65.9237039528771,-1.63165946910082,8.07283920347654));
#22195=CARTESIAN_POINT('Ctrl Pts',(65.9237039528771,-4.03165946910082,8.07283920347654));
#22196=CARTESIAN_POINT('Ctrl Pts',(66.6557369297143,-1.63165946910082,8.28958012503506));
#22197=CARTESIAN_POINT('Ctrl Pts',(66.6557369297143,-4.03165946910082,8.28958012503506));
#22198=CARTESIAN_POINT('Ctrl Pts',(67.3150092482541,-1.63165946910082,8.50886642156035));
#22199=CARTESIAN_POINT('Ctrl Pts',(67.3150092482541,-4.03165946910082,8.50886642156035));
#22200=CARTESIAN_POINT('Ctrl Pts',(67.8492602326033,-1.63165946910082,8.69890399191606));
#22201=CARTESIAN_POINT('Ctrl Pts',(67.8492602326033,-4.03165946910082,8.69890399191606));
#22202=CARTESIAN_POINT('Ctrl Pts',(68.2198703338295,-1.63165946910082,8.83566471550562));
#22203=CARTESIAN_POINT('Ctrl Pts',(68.2198703338295,-4.03165946910082,8.83566471550562));
#22204=CARTESIAN_POINT('Ctrl Pts',(68.403087843053,-1.63165946910082,8.90436665637972));
#22205=CARTESIAN_POINT('Ctrl Pts',(68.403087843053,-4.03165946910082,8.90436665637972));
#22206=CARTESIAN_POINT('',(34.5886335096989,-1.63165946910082,1.82713536652871));
#22207=CARTESIAN_POINT('Origin',(32.143405418954,-1.63165946910082,3.2164639050219));
#22208=CARTESIAN_POINT('',(30.067343367632,-1.63165946910082,1.31927109386626));
#22209=CARTESIAN_POINT('Origin',(25.6749565963595,-1.63165946910082,-3.12914171551276));
#22210=CARTESIAN_POINT('',(25.3459666144763,-1.63165946910082,3.11371049024365));
#22211=CARTESIAN_POINT('Origin',(24.7143466872546,-1.63165946910082,5.90470262206354));
#22212=CARTESIAN_POINT('',(0.,0.,0.));
#22213=CARTESIAN_POINT('Ctrl Pts',(13.9521549326808,4.33051922028271,-3.));
#22214=CARTESIAN_POINT('Ctrl Pts',(13.9521549326808,4.33051922028271,11.4));
#22215=CARTESIAN_POINT('Ctrl Pts',(14.0367700658778,4.33051922028271,-3.));
#22216=CARTESIAN_POINT('Ctrl Pts',(14.0367700658778,4.33051922028271,11.4));
#22217=CARTESIAN_POINT('Ctrl Pts',(14.2036369078635,4.3237071977066,-3.));
#22218=CARTESIAN_POINT('Ctrl Pts',(14.2036369078635,4.3237071977066,11.4));
#22219=CARTESIAN_POINT('Ctrl Pts',(14.4468469322399,4.29305314840303,-3.));
#22220=CARTESIAN_POINT('Ctrl Pts',(14.4468469322399,4.29305314840303,11.4));
#22221=CARTESIAN_POINT('Ctrl Pts',(14.7569409494257,4.21100033264776,-3.));
#22222=CARTESIAN_POINT('Ctrl Pts',(14.7569409494257,4.21100033264776,11.4));
#22223=CARTESIAN_POINT('Ctrl Pts',(15.1212896693278,4.03949049111154,-3.));
#22224=CARTESIAN_POINT('Ctrl Pts',(15.1212896693278,4.03949049111154,11.4));
#22225=CARTESIAN_POINT('Ctrl Pts',(15.4636185066764,3.80138932605477,-3.));
#22226=CARTESIAN_POINT('Ctrl Pts',(15.4636185066764,3.80138932605477,11.4));
#22227=CARTESIAN_POINT('Ctrl Pts',(15.7866049591328,3.50410652905647,-3.));
#22228=CARTESIAN_POINT('Ctrl Pts',(15.7866049591328,3.50410652905647,11.4));
#22229=CARTESIAN_POINT('Ctrl Pts',(16.0950135392462,3.16285055044176,-3.));
#22230=CARTESIAN_POINT('Ctrl Pts',(16.0950135392462,3.16285055044176,11.4));
#22231=CARTESIAN_POINT('Ctrl Pts',(16.396392567999,2.80347808583323,-3.));
#22232=CARTESIAN_POINT('Ctrl Pts',(16.396392567999,2.80347808583323,11.4));
#22233=CARTESIAN_POINT('Ctrl Pts',(16.6994685020962,2.45665970286042,-3.));
#22234=CARTESIAN_POINT('Ctrl Pts',(16.6994685020962,2.45665970286042,11.4));
#22235=CARTESIAN_POINT('Ctrl Pts',(17.0126841408516,2.15256650575318,-3.));
#22236=CARTESIAN_POINT('Ctrl Pts',(17.0126841408516,2.15256650575318,11.4));
#22237=CARTESIAN_POINT('Ctrl Pts',(17.3426063821155,1.91508101584403,-3.));
#22238=CARTESIAN_POINT('Ctrl Pts',(17.3426063821155,1.91508101584403,11.4));
#22239=CARTESIAN_POINT('Ctrl Pts',(17.6925082784732,1.75662630260534,-3.));
#22240=CARTESIAN_POINT('Ctrl Pts',(17.6925082784732,1.75662630260534,11.4));
#22241=CARTESIAN_POINT('Ctrl Pts',(18.0602469444161,1.6704655276535,-3.));
#22242=CARTESIAN_POINT('Ctrl Pts',(18.0602469444161,1.6704655276535,11.4));
#22243=CARTESIAN_POINT('Ctrl Pts',(18.4399535686149,1.63662374391445,-3.));
#22244=CARTESIAN_POINT('Ctrl Pts',(18.4399535686149,1.63662374391445,11.4));
#22245=CARTESIAN_POINT('Ctrl Pts',(18.7476534820197,1.63200385678456,-3.));
#22246=CARTESIAN_POINT('Ctrl Pts',(18.7476534820197,1.63200385678456,11.4));
#22247=CARTESIAN_POINT('Ctrl Pts',(18.9779068684107,1.63172180635354,-3.));
#22248=CARTESIAN_POINT('Ctrl Pts',(18.9779068684107,1.63172180635354,11.4));
#22249=CARTESIAN_POINT('Ctrl Pts',(19.1308048362197,1.63165946910082,-3.));
#22250=CARTESIAN_POINT('Ctrl Pts',(19.1308048362197,1.63165946910082,11.4));
#22251=CARTESIAN_POINT('Ctrl Pts',(19.2071026744088,1.63165946910082,-3.));
#22252=CARTESIAN_POINT('Ctrl Pts',(19.2071026744088,1.63165946910082,11.4));
#22253=CARTESIAN_POINT('',(13.9521549326808,4.33051922028271,-0.737782898536615));
#22254=CARTESIAN_POINT('',(19.2071026744088,1.63165946910082,-0.737782898536615));
#22255=CARTESIAN_POINT('Ctrl Pts',(13.9521549326808,4.33051922028271,-0.737782898536615));
#22256=CARTESIAN_POINT('Ctrl Pts',(14.0367700658778,4.33051922028271,-0.737782898536615));
#22257=CARTESIAN_POINT('Ctrl Pts',(14.2036369078635,4.3237071977066,-0.737782898536615));
#22258=CARTESIAN_POINT('Ctrl Pts',(14.4468469322399,4.29305314840303,-0.737782898536615));
#22259=CARTESIAN_POINT('Ctrl Pts',(14.7569409494257,4.21100033264776,-0.737782898536615));
#22260=CARTESIAN_POINT('Ctrl Pts',(15.1212896693278,4.03949049111154,-0.737782898536615));
#22261=CARTESIAN_POINT('Ctrl Pts',(15.4636185066764,3.80138932605477,-0.737782898536615));
#22262=CARTESIAN_POINT('Ctrl Pts',(15.7866049591328,3.50410652905647,-0.737782898536615));
#22263=CARTESIAN_POINT('Ctrl Pts',(16.0950135392462,3.16285055044176,-0.737782898536615));
#22264=CARTESIAN_POINT('Ctrl Pts',(16.396392567999,2.80347808583323,-0.737782898536615));
#22265=CARTESIAN_POINT('Ctrl Pts',(16.6994685020962,2.45665970286042,-0.737782898536615));
#22266=CARTESIAN_POINT('Ctrl Pts',(17.0126841408516,2.15256650575318,-0.737782898536615));
#22267=CARTESIAN_POINT('Ctrl Pts',(17.3426063821155,1.91508101584403,-0.737782898536615));
#22268=CARTESIAN_POINT('Ctrl Pts',(17.6925082784732,1.75662630260534,-0.737782898536615));
#22269=CARTESIAN_POINT('Ctrl Pts',(18.0602469444161,1.6704655276535,-0.737782898536615));
#22270=CARTESIAN_POINT('Ctrl Pts',(18.4399535686149,1.63662374391445,-0.737782898536615));
#22271=CARTESIAN_POINT('Ctrl Pts',(18.7476534820197,1.63200385678456,-0.737782898536615));
#22272=CARTESIAN_POINT('Ctrl Pts',(18.9779068684107,1.63172180635354,-0.737782898536615));
#22273=CARTESIAN_POINT('Ctrl Pts',(19.1308048362197,1.63165946910082,-0.737782898536615));
#22274=CARTESIAN_POINT('Ctrl Pts',(19.2071026744088,1.63165946910082,-0.737782898536615));
#22275=CARTESIAN_POINT('',(13.9521549326808,4.33051922028271,5.59936274946018));
#22276=CARTESIAN_POINT('',(13.9521549326808,4.33051922028271,0.));
#22277=CARTESIAN_POINT('',(19.2071026744088,1.63165946910082,5.59936274946018));
#22278=CARTESIAN_POINT('Ctrl Pts',(19.2071026744088,1.63165946910082,5.59936274946018));
#22279=CARTESIAN_POINT('Ctrl Pts',(19.1308048362197,1.63165946910082,5.59936274946018));
#22280=CARTESIAN_POINT('Ctrl Pts',(18.9779068684107,1.63172180635354,5.59936274946018));
#22281=CARTESIAN_POINT('Ctrl Pts',(18.7476534820197,1.63200385678456,5.59936274946018));
#22282=CARTESIAN_POINT('Ctrl Pts',(18.4399535686149,1.63662374391445,5.59936274946018));
#22283=CARTESIAN_POINT('Ctrl Pts',(18.0602469444161,1.6704655276535,5.59936274946018));
#22284=CARTESIAN_POINT('Ctrl Pts',(17.6925082784732,1.75662630260534,5.59936274946018));
#22285=CARTESIAN_POINT('Ctrl Pts',(17.3426063821155,1.91508101584403,5.59936274946018));
#22286=CARTESIAN_POINT('Ctrl Pts',(17.0126841408516,2.15256650575318,5.59936274946018));
#22287=CARTESIAN_POINT('Ctrl Pts',(16.6994685020962,2.45665970286042,5.59936274946018));
#22288=CARTESIAN_POINT('Ctrl Pts',(16.396392567999,2.80347808583323,5.59936274946018));
#22289=CARTESIAN_POINT('Ctrl Pts',(16.0950135392462,3.16285055044176,5.59936274946018));
#22290=CARTESIAN_POINT('Ctrl Pts',(15.7866049591328,3.50410652905647,5.59936274946018));
#22291=CARTESIAN_POINT('Ctrl Pts',(15.4636185066764,3.80138932605477,5.59936274946018));
#22292=CARTESIAN_POINT('Ctrl Pts',(15.1212896693278,4.03949049111154,5.59936274946018));
#22293=CARTESIAN_POINT('Ctrl Pts',(14.7569409494257,4.21100033264776,5.59936274946018));
#22294=CARTESIAN_POINT('Ctrl Pts',(14.4468469322399,4.29305314840303,5.59936274946018));
#22295=CARTESIAN_POINT('Ctrl Pts',(14.2036369078635,4.3237071977066,5.59936274946018));
#22296=CARTESIAN_POINT('Ctrl Pts',(14.0367700658778,4.33051922028271,5.59936274946018));
#22297=CARTESIAN_POINT('Ctrl Pts',(13.9521549326808,4.33051922028271,5.59936274946018));
#22298=CARTESIAN_POINT('',(19.2071026744088,1.63165946910082,0.));
#22299=CARTESIAN_POINT('Ctrl Pts',(19.2071026744088,-0.0183405308991755,
-3.01914151387231));
#22300=CARTESIAN_POINT('Ctrl Pts',(19.2071026744088,-0.0183405308991755,
11.4038283027745));
#22301=CARTESIAN_POINT('Ctrl Pts',(18.932554067018,-0.0183405308991755,
-3.01914151387231));
#22302=CARTESIAN_POINT('Ctrl Pts',(18.932554067018,-0.0183405308991755,
11.4038283027745));
#22303=CARTESIAN_POINT('Ctrl Pts',(18.6452346172082,-0.0244648993437209,
-3.01914151387231));
#22304=CARTESIAN_POINT('Ctrl Pts',(18.6452346172082,-0.0244648993437209,
11.4038283027745));
#22305=CARTESIAN_POINT('Ctrl Pts',(18.2737554003772,0.00094178007888357,
-3.01914151387231));
#22306=CARTESIAN_POINT('Ctrl Pts',(18.2737554003772,0.00094178007888357,
11.4038283027745));
#22307=CARTESIAN_POINT('Ctrl Pts',(17.815024722384,0.0323158724884442,-3.01914151387231));
#22308=CARTESIAN_POINT('Ctrl Pts',(17.815024722384,0.0323158724884442,11.4038283027745));
#22309=CARTESIAN_POINT('Ctrl Pts',(17.2029954141084,0.14276585350144,-3.01914151387231));
#22310=CARTESIAN_POINT('Ctrl Pts',(17.2029954141084,0.14276585350144,11.4038283027745));
#22311=CARTESIAN_POINT('Ctrl Pts',(16.6476240631459,0.436436950410268,-3.01914151387231));
#22312=CARTESIAN_POINT('Ctrl Pts',(16.6476240631459,0.436436950410268,11.4038283027745));
#22313=CARTESIAN_POINT('Ctrl Pts',(16.0510567137341,0.751891803416538,-3.01914151387231));
#22314=CARTESIAN_POINT('Ctrl Pts',(16.0510567137341,0.751891803416538,11.4038283027745));
#22315=CARTESIAN_POINT('Ctrl Pts',(15.6027736445726,1.21202503656501,-3.01914151387231));
#22316=CARTESIAN_POINT('Ctrl Pts',(15.6027736445726,1.21202503656501,11.4038283027745));
#22317=CARTESIAN_POINT('Ctrl Pts',(15.2713584598603,1.58690028117533,-3.01914151387231));
#22318=CARTESIAN_POINT('Ctrl Pts',(15.2713584598603,1.58690028117533,11.4038283027745));
#22319=CARTESIAN_POINT('Ctrl Pts',(14.8456161221497,2.0684722499697,-3.01914151387231));
#22320=CARTESIAN_POINT('Ctrl Pts',(14.8456161221497,2.0684722499697,11.4038283027745));
#22321=CARTESIAN_POINT('Ctrl Pts',(14.5613685394243,2.40143629916816,-3.01914151387231));
#22322=CARTESIAN_POINT('Ctrl Pts',(14.5613685394243,2.40143629916816,11.4038283027745));
#22323=CARTESIAN_POINT('Ctrl Pts',(14.3828812435025,2.53302458721095,-3.01914151387231));
#22324=CARTESIAN_POINT('Ctrl Pts',(14.3828812435025,2.53302458721095,11.4038283027745));
#22325=CARTESIAN_POINT('Ctrl Pts',(14.201535511025,2.66672023404866,-3.01914151387231));
#22326=CARTESIAN_POINT('Ctrl Pts',(14.201535511025,2.66672023404866,11.4038283027745));
#22327=CARTESIAN_POINT('Ctrl Pts',(14.14690312219,2.68051922028271,-3.01914151387231));
#22328=CARTESIAN_POINT('Ctrl Pts',(14.14690312219,2.68051922028271,11.4038283027745));
#22329=CARTESIAN_POINT('Ctrl Pts',(13.9521549326808,2.68051922028271,-3.01914151387231));
#22330=CARTESIAN_POINT('Ctrl Pts',(13.9521549326808,2.68051922028271,11.4038283027745));
#22331=CARTESIAN_POINT('',(18.2877550231844,1.59204426907891E-25,5.59936274946018));
#22332=CARTESIAN_POINT('',(18.2877550231844,-7.96022134539453E-26,-0.737782898536615));
#22333=CARTESIAN_POINT('',(18.2877582116991,5.55111512312578E-16,5.59936274946018));
#22334=CARTESIAN_POINT('',(13.9521549326808,2.68051922028271,5.59936274946018));
#22335=CARTESIAN_POINT('Ctrl Pts',(13.9521549326808,2.68051922028271,5.59936274946018));
#22336=CARTESIAN_POINT('Ctrl Pts',(14.14690312219,2.68051922028271,5.59936274946018));
#22337=CARTESIAN_POINT('Ctrl Pts',(14.201535511025,2.66672023404866,5.59936274946018));
#22338=CARTESIAN_POINT('Ctrl Pts',(14.3828812435025,2.53302458721095,5.59936274946018));
#22339=CARTESIAN_POINT('Ctrl Pts',(14.5613685394243,2.40143629916816,5.59936274946018));
#22340=CARTESIAN_POINT('Ctrl Pts',(14.8456161221497,2.0684722499697,5.59936274946018));
#22341=CARTESIAN_POINT('Ctrl Pts',(15.2713584598603,1.58690028117533,5.59936274946018));
#22342=CARTESIAN_POINT('Ctrl Pts',(15.6027736445726,1.21202503656501,5.59936274946018));
#22343=CARTESIAN_POINT('Ctrl Pts',(16.0510567137341,0.751891803416538,5.59936274946018));
#22344=CARTESIAN_POINT('Ctrl Pts',(16.6476240631459,0.436436950410268,5.59936274946018));
#22345=CARTESIAN_POINT('Ctrl Pts',(17.2029954141084,0.14276585350144,5.59936274946018));
#22346=CARTESIAN_POINT('Ctrl Pts',(17.815024722384,0.0323158724884442,5.59936274946018));
#22347=CARTESIAN_POINT('Ctrl Pts',(18.2737554003772,0.00094178007888357,
5.59936274946018));
#22348=CARTESIAN_POINT('Ctrl Pts',(18.2784351727308,0.000621715131582291,
5.59936274946018));
#22349=CARTESIAN_POINT('Ctrl Pts',(18.2831015888222,0.000306654201738636,
5.59936274946018));
#22350=CARTESIAN_POINT('Ctrl Pts',(18.2877547913768,-3.47799384755541E-6,
5.59936274946018));
#22351=CARTESIAN_POINT('',(13.9521549326808,2.68051922028271,-0.737782898536615));
#22352=CARTESIAN_POINT('',(13.9521549326808,2.68051922028271,0.));
#22353=CARTESIAN_POINT('Ctrl Pts',(18.2877536206758,-3.39996748941005E-6,
-0.737782898536615));
#22354=CARTESIAN_POINT('Ctrl Pts',(18.2831008061387,0.000306707045957792,
-0.737782898536615));
#22355=CARTESIAN_POINT('Ctrl Pts',(18.278434780269,0.000621741973328407,
-0.737782898536615));
#22356=CARTESIAN_POINT('Ctrl Pts',(17.815024722384,0.0323158724884443,-0.737782898536615));
#22357=CARTESIAN_POINT('Ctrl Pts',(17.2029954141084,0.14276585350144,-0.737782898536615));
#22358=CARTESIAN_POINT('Ctrl Pts',(16.0510567137341,0.751891803416538,-0.737782898536615));
#22359=CARTESIAN_POINT('Ctrl Pts',(15.6027736445726,1.21202503656501,-0.737782898536615));
#22360=CARTESIAN_POINT('Ctrl Pts',(14.8456161221497,2.0684722499697,-0.737782898536615));
#22361=CARTESIAN_POINT('Ctrl Pts',(14.5613685394243,2.40143629916816,-0.737782898536615));
#22362=CARTESIAN_POINT('Ctrl Pts',(14.201535511025,2.66672023404866,-0.737782898536615));
#22363=CARTESIAN_POINT('Ctrl Pts',(14.14690312219,2.68051922028271,-0.737782898536615));
#22364=CARTESIAN_POINT('Ctrl Pts',(13.9521549326808,2.68051922028271,-0.737782898536615));
#22365=CARTESIAN_POINT('Origin',(19.2071026744088,1.63165946910082,0.));
#22366=CARTESIAN_POINT('',(25.8992960798277,1.63165946910082,-3.));
#22367=CARTESIAN_POINT('',(27.575916328613,1.63165946910082,-0.395297377936459));
#22368=CARTESIAN_POINT('Origin',(24.7143466872546,1.63165946910082,-0.395297377936459));
#22369=CARTESIAN_POINT('',(23.5207683417462,1.63165946910082,-3.));
#22370=CARTESIAN_POINT('',(19.2071026744088,1.63165946910082,-3.));
#22371=CARTESIAN_POINT('',(20.1650770882888,1.63165946910082,-0.737782898536615));
#22372=CARTESIAN_POINT('Ctrl Pts',(20.1650770882888,1.63165946910083,-0.737782898536615));
#22373=CARTESIAN_POINT('Ctrl Pts',(20.2051790492699,1.63165946910083,-0.737782898536615));
#22374=CARTESIAN_POINT('Ctrl Pts',(20.2856318058959,1.63165946910083,-0.738334262610078));
#22375=CARTESIAN_POINT('Ctrl Pts',(20.4070574409421,1.63165946910083,-0.740817279017836));
#22376=CARTESIAN_POINT('Ctrl Pts',(20.570466834294,1.63165946910083,-0.750031355028731));
#22377=CARTESIAN_POINT('Ctrl Pts',(20.7773607278973,1.63165946910083,-0.785302229564316));
#22378=CARTESIAN_POINT('Ctrl Pts',(20.9870805449298,1.63165946910083,-0.859882777793607));
#22379=CARTESIAN_POINT('Ctrl Pts',(21.1998878964781,1.63165946910083,-0.985918438087056));
#22380=CARTESIAN_POINT('Ctrl Pts',(21.4160984502468,1.63165946910083,-1.16513193018819));
#22381=CARTESIAN_POINT('Ctrl Pts',(21.6360629244597,1.63165946910083,-1.38851558520595));
#22382=CARTESIAN_POINT('Ctrl Pts',(21.8601428560791,1.63165946910083,-1.64103427806176));
#22383=CARTESIAN_POINT('Ctrl Pts',(22.0886743686473,1.63165946910083,-1.90460559759654));
#22384=CARTESIAN_POINT('Ctrl Pts',(22.3219273279567,1.63165946910083,-2.16140314464429));
#22385=CARTESIAN_POINT('Ctrl Pts',(22.5600378010161,1.63165946910083,-2.3973000769867));
#22386=CARTESIAN_POINT('Ctrl Pts',(22.8029682104327,1.63165946910083,-2.60422537589526));
#22387=CARTESIAN_POINT('Ctrl Pts',(23.0429827907474,1.63165946910083,-2.77271153031038));
#22388=CARTESIAN_POINT('Ctrl Pts',(23.2368431253681,1.63165946910083,-2.88095209536456));
#22389=CARTESIAN_POINT('Ctrl Pts',(23.3821028186482,1.63165946910083,-2.94712138325619));
#22390=CARTESIAN_POINT('Ctrl Pts',(23.4770787559704,1.63165946910083,-2.98421892689512));
#22391=CARTESIAN_POINT('Ctrl Pts',(23.5207683417462,1.63165946910083,-3.));
#22392=CARTESIAN_POINT('',(8.65639871597966,1.63165946910082,-0.737782898536615));
#22393=CARTESIAN_POINT('',(20.1650770882888,1.63165946910082,5.59936274946018));
#22394=CARTESIAN_POINT('',(19.6860898813488,1.63165946910082,5.59936274946018));
#22395=CARTESIAN_POINT('',(21.9988718582129,1.63165946910082,6.80735275649273));
#22396=CARTESIAN_POINT('Origin',(20.1650770882888,1.63165946910082,7.59525803303831));
#22397=CARTESIAN_POINT('',(27.575916328613,1.63165946910082,5.90470262206354));
#22398=CARTESIAN_POINT('Origin',(24.7143466872546,1.63165946910082,5.90470262206354));
#22399=CARTESIAN_POINT('',(27.575916328613,1.63165946910082,0.));
#22400=CARTESIAN_POINT('',(23.013011518287,1.63165946910082,5.90470262206354));
#22401=CARTESIAN_POINT('Origin',(24.7143466872546,1.63165946910082,5.90470262206354));
#22402=CARTESIAN_POINT('',(23.013011518287,1.63165946910082,-0.395297377936459));
#22403=CARTESIAN_POINT('Origin',(24.7143466872546,1.63165946910082,-0.395297377936459));
#22404=CARTESIAN_POINT('Origin',(5.09382715545311,4.33051922028271,0.));
#22405=CARTESIAN_POINT('',(5.09382715545311,4.33051922028271,-0.737782898536615));
#22406=CARTESIAN_POINT('',(1.59976095650181,4.33051922028271,-0.737782898536615));
#22407=CARTESIAN_POINT('',(5.09382715545311,4.33051922028271,5.59936274946018));
#22408=CARTESIAN_POINT('',(5.09382715545311,4.33051922028271,0.));
#22409=CARTESIAN_POINT('',(12.629452121871,4.33051922028271,5.59936274946018));
#22410=CARTESIAN_POINT('Origin',(5.1457717363639,2.68051922028271,0.));
#22411=CARTESIAN_POINT('',(5.1457717363639,2.68051922028271,-0.737782898536615));
#22412=CARTESIAN_POINT('',(5.1457717363639,2.6650130345292,-0.737782898536615));
#22413=CARTESIAN_POINT('',(5.1457717363639,1.34025961014136,-0.737782898536615));
#22414=CARTESIAN_POINT('',(5.1457717363639,2.68051922028271,5.59936274946018));
#22415=CARTESIAN_POINT('',(5.1457717363639,2.68051922028271,0.));
#22416=CARTESIAN_POINT('',(5.1457717363639,2.6650130345292,5.59936274946018));
#22417=CARTESIAN_POINT('',(5.1457717363639,1.34025961014136,5.59936274946018));
#22418=CARTESIAN_POINT('',(5.1457717363639,2.6650130345292,0.));
#22419=CARTESIAN_POINT('Origin',(13.9521549326808,2.68051922028271,0.));
#22420=CARTESIAN_POINT('',(6.02892484511565,2.68051922028271,-0.737782898536615));
#22421=CARTESIAN_POINT('',(17.0586160104848,2.68051922028271,5.59936274946018));
#22422=CARTESIAN_POINT('Ctrl Pts',(19.2071026744088,0.0183405308991755,
-3.01914151387231));
#22423=CARTESIAN_POINT('Ctrl Pts',(19.2071026744088,0.0183405308991755,
11.4038283027745));
#22424=CARTESIAN_POINT('Ctrl Pts',(18.932554067018,0.0183405308991755,-3.01914151387231));
#22425=CARTESIAN_POINT('Ctrl Pts',(18.932554067018,0.0183405308991755,11.4038283027745));
#22426=CARTESIAN_POINT('Ctrl Pts',(18.6452346172082,0.0244648993437209,
-3.01914151387231));
#22427=CARTESIAN_POINT('Ctrl Pts',(18.6452346172082,0.0244648993437209,
11.4038283027745));
#22428=CARTESIAN_POINT('Ctrl Pts',(18.2737554003772,-0.00094178007888357,
-3.01914151387231));
#22429=CARTESIAN_POINT('Ctrl Pts',(18.2737554003772,-0.00094178007888357,
11.4038283027745));
#22430=CARTESIAN_POINT('Ctrl Pts',(17.815024722384,-0.0323158724884442,
-3.01914151387231));
#22431=CARTESIAN_POINT('Ctrl Pts',(17.815024722384,-0.0323158724884442,
11.4038283027745));
#22432=CARTESIAN_POINT('Ctrl Pts',(17.2029954141084,-0.14276585350144,-3.01914151387231));
#22433=CARTESIAN_POINT('Ctrl Pts',(17.2029954141084,-0.14276585350144,11.4038283027745));
#22434=CARTESIAN_POINT('Ctrl Pts',(16.6476240631459,-0.436436950410268,
-3.01914151387231));
#22435=CARTESIAN_POINT('Ctrl Pts',(16.6476240631459,-0.436436950410268,
11.4038283027745));
#22436=CARTESIAN_POINT('Ctrl Pts',(16.0510567137341,-0.751891803416538,
-3.01914151387231));
#22437=CARTESIAN_POINT('Ctrl Pts',(16.0510567137341,-0.751891803416538,
11.4038283027745));
#22438=CARTESIAN_POINT('Ctrl Pts',(15.6027736445726,-1.21202503656501,-3.01914151387231));
#22439=CARTESIAN_POINT('Ctrl Pts',(15.6027736445726,-1.21202503656501,11.4038283027745));
#22440=CARTESIAN_POINT('Ctrl Pts',(15.2713584598603,-1.58690028117533,-3.01914151387231));
#22441=CARTESIAN_POINT('Ctrl Pts',(15.2713584598603,-1.58690028117533,11.4038283027745));
#22442=CARTESIAN_POINT('Ctrl Pts',(14.8456161221497,-2.0684722499697,-3.01914151387231));
#22443=CARTESIAN_POINT('Ctrl Pts',(14.8456161221497,-2.0684722499697,11.4038283027745));
#22444=CARTESIAN_POINT('Ctrl Pts',(14.5613685394243,-2.40143629916816,-3.01914151387231));
#22445=CARTESIAN_POINT('Ctrl Pts',(14.5613685394243,-2.40143629916816,11.4038283027745));
#22446=CARTESIAN_POINT('Ctrl Pts',(14.3828812435025,-2.53302458721095,-3.01914151387231));
#22447=CARTESIAN_POINT('Ctrl Pts',(14.3828812435025,-2.53302458721095,11.4038283027745));
#22448=CARTESIAN_POINT('Ctrl Pts',(14.201535511025,-2.66672023404866,-3.01914151387231));
#22449=CARTESIAN_POINT('Ctrl Pts',(14.201535511025,-2.66672023404866,11.4038283027745));
#22450=CARTESIAN_POINT('Ctrl Pts',(14.14690312219,-2.68051922028271,-3.01914151387231));
#22451=CARTESIAN_POINT('Ctrl Pts',(14.14690312219,-2.68051922028271,11.4038283027745));
#22452=CARTESIAN_POINT('Ctrl Pts',(13.9521549326808,-2.68051922028271,-3.01914151387231));
#22453=CARTESIAN_POINT('Ctrl Pts',(13.9521549326808,-2.68051922028271,11.4038283027745));
#22454=CARTESIAN_POINT('',(13.9521549326808,-2.68051922028271,-0.737782898536615));
#22455=CARTESIAN_POINT('Ctrl Pts',(18.2877536206758,3.39996748803095E-6,
-0.737782898536615));
#22456=CARTESIAN_POINT('Ctrl Pts',(18.2831008061387,-0.000306707045958711,
-0.737782898536615));
#22457=CARTESIAN_POINT('Ctrl Pts',(18.278434780269,-0.000621741973328828,
-0.737782898536615));
#22458=CARTESIAN_POINT('Ctrl Pts',(17.815024722384,-0.0323158724884442,
-0.737782898536615));
#22459=CARTESIAN_POINT('Ctrl Pts',(17.2029954141084,-0.14276585350144,-0.737782898536615));
#22460=CARTESIAN_POINT('Ctrl Pts',(16.0510567137341,-0.751891803416538,
-0.737782898536615));
#22461=CARTESIAN_POINT('Ctrl Pts',(15.6027736445726,-1.21202503656501,-0.737782898536615));
#22462=CARTESIAN_POINT('Ctrl Pts',(14.8456161221497,-2.0684722499697,-0.737782898536615));
#22463=CARTESIAN_POINT('Ctrl Pts',(14.5613685394243,-2.40143629916816,-0.737782898536615));
#22464=CARTESIAN_POINT('Ctrl Pts',(14.201535511025,-2.66672023404866,-0.737782898536615));
#22465=CARTESIAN_POINT('Ctrl Pts',(14.14690312219,-2.68051922028271,-0.737782898536615));
#22466=CARTESIAN_POINT('Ctrl Pts',(13.9521549326808,-2.68051922028271,-0.737782898536615));
#22467=CARTESIAN_POINT('',(13.9521549326808,-2.68051922028271,5.59936274946018));
#22468=CARTESIAN_POINT('',(13.9521549326808,-2.68051922028271,0.));
#22469=CARTESIAN_POINT('Ctrl Pts',(13.9521549326808,-2.68051922028271,5.59936274946018));
#22470=CARTESIAN_POINT('Ctrl Pts',(14.14690312219,-2.68051922028271,5.59936274946018));
#22471=CARTESIAN_POINT('Ctrl Pts',(14.201535511025,-2.66672023404866,5.59936274946018));
#22472=CARTESIAN_POINT('Ctrl Pts',(14.3828812435025,-2.53302458721095,5.59936274946018));
#22473=CARTESIAN_POINT('Ctrl Pts',(14.5613685394243,-2.40143629916816,5.59936274946018));
#22474=CARTESIAN_POINT('Ctrl Pts',(14.8456161221497,-2.0684722499697,5.59936274946018));
#22475=CARTESIAN_POINT('Ctrl Pts',(15.2713584598603,-1.58690028117533,5.59936274946018));
#22476=CARTESIAN_POINT('Ctrl Pts',(15.6027736445726,-1.21202503656501,5.59936274946018));
#22477=CARTESIAN_POINT('Ctrl Pts',(16.0510567137341,-0.751891803416538,
5.59936274946018));
#22478=CARTESIAN_POINT('Ctrl Pts',(16.6476240631459,-0.436436950410268,
5.59936274946018));
#22479=CARTESIAN_POINT('Ctrl Pts',(17.2029954141084,-0.14276585350144,5.59936274946018));
#22480=CARTESIAN_POINT('Ctrl Pts',(17.815024722384,-0.0323158724884442,
5.59936274946018));
#22481=CARTESIAN_POINT('Ctrl Pts',(18.2737554003772,-0.00094178007888357,
5.59936274946018));
#22482=CARTESIAN_POINT('Ctrl Pts',(18.2784351727308,-0.000621715131582311,
5.59936274946018));
#22483=CARTESIAN_POINT('Ctrl Pts',(18.2831015888222,-0.000306654201738675,
5.59936274946018));
#22484=CARTESIAN_POINT('Ctrl Pts',(18.2877547913768,3.477993847498E-6,5.59936274946018));
#22485=CARTESIAN_POINT('Origin',(-1.89430524244949,0.,-0.737782898536615));
#22486=CARTESIAN_POINT('',(20.1650770882888,-1.63165946910082,-0.737782898536615));
#22487=CARTESIAN_POINT('',(20.1650770882888,0.,-0.737782898536615));
#22488=CARTESIAN_POINT('',(19.2071026744088,-1.63165946910082,-0.737782898536615));
#22489=CARTESIAN_POINT('',(8.65639871597966,-1.63165946910082,-0.737782898536615));
#22490=CARTESIAN_POINT('',(13.9521549326808,-4.33051922028271,-0.737782898536615));
#22491=CARTESIAN_POINT('Ctrl Pts',(13.9521549326808,-4.33051922028271,-0.737782898536615));
#22492=CARTESIAN_POINT('Ctrl Pts',(14.0367700658778,-4.33051922028271,-0.737782898536615));
#22493=CARTESIAN_POINT('Ctrl Pts',(14.2036369078635,-4.3237071977066,-0.737782898536615));
#22494=CARTESIAN_POINT('Ctrl Pts',(14.4468469322399,-4.29305314840303,-0.737782898536615));
#22495=CARTESIAN_POINT('Ctrl Pts',(14.7569409494257,-4.21100033264776,-0.737782898536615));
#22496=CARTESIAN_POINT('Ctrl Pts',(15.1212896693278,-4.03949049111154,-0.737782898536615));
#22497=CARTESIAN_POINT('Ctrl Pts',(15.4636185066764,-3.80138932605477,-0.737782898536615));
#22498=CARTESIAN_POINT('Ctrl Pts',(15.7866049591328,-3.50410652905647,-0.737782898536615));
#22499=CARTESIAN_POINT('Ctrl Pts',(16.0950135392462,-3.16285055044176,-0.737782898536615));
#22500=CARTESIAN_POINT('Ctrl Pts',(16.396392567999,-2.80347808583323,-0.737782898536615));
#22501=CARTESIAN_POINT('Ctrl Pts',(16.6994685020962,-2.45665970286042,-0.737782898536615));
#22502=CARTESIAN_POINT('Ctrl Pts',(17.0126841408516,-2.15256650575318,-0.737782898536615));
#22503=CARTESIAN_POINT('Ctrl Pts',(17.3426063821155,-1.91508101584403,-0.737782898536615));
#22504=CARTESIAN_POINT('Ctrl Pts',(17.6925082784732,-1.75662630260534,-0.737782898536615));
#22505=CARTESIAN_POINT('Ctrl Pts',(18.0602469444161,-1.6704655276535,-0.737782898536615));
#22506=CARTESIAN_POINT('Ctrl Pts',(18.4399535686149,-1.63662374391445,-0.737782898536615));
#22507=CARTESIAN_POINT('Ctrl Pts',(18.7476534820197,-1.63200385678456,-0.737782898536615));
#22508=CARTESIAN_POINT('Ctrl Pts',(18.9779068684107,-1.63172180635354,-0.737782898536615));
#22509=CARTESIAN_POINT('Ctrl Pts',(19.1308048362197,-1.63165946910082,-0.737782898536615));
#22510=CARTESIAN_POINT('Ctrl Pts',(19.2071026744088,-1.63165946910082,-0.737782898536615));
#22511=CARTESIAN_POINT('',(5.09382715545311,-4.33051922028271,-0.737782898536615));
#22512=CARTESIAN_POINT('',(1.59976095650181,-4.33051922028271,-0.737782898536615));
#22513=CARTESIAN_POINT('Origin',(5.09382715545311,0.,-0.737782898536615));
#22514=CARTESIAN_POINT('',(5.1457717363639,-2.6650130345292,-0.737782898536615));
#22515=CARTESIAN_POINT('Origin',(5.09382715545311,0.,-0.737782898536615));
#22516=CARTESIAN_POINT('',(5.1457717363639,-2.68051922028271,-0.737782898536615));
#22517=CARTESIAN_POINT('',(5.1457717363639,-1.34025961014136,-0.737782898536615));
#22518=CARTESIAN_POINT('',(6.02892484511565,-2.68051922028271,-0.737782898536615));
#22519=CARTESIAN_POINT('Ctrl Pts',(20.1650770882888,-12.,-0.737782898536615));
#22520=CARTESIAN_POINT('Ctrl Pts',(20.1650770882888,16.8,-0.737782898536615));
#22521=CARTESIAN_POINT('Ctrl Pts',(20.2051790492699,-12.,-0.737782898536615));
#22522=CARTESIAN_POINT('Ctrl Pts',(20.2051790492699,16.8,-0.737782898536615));
#22523=CARTESIAN_POINT('Ctrl Pts',(20.2856318058959,-12.,-0.738334262610078));
#22524=CARTESIAN_POINT('Ctrl Pts',(20.2856318058959,16.8,-0.738334262610078));
#22525=CARTESIAN_POINT('Ctrl Pts',(20.4070574409421,-12.,-0.740817279017836));
#22526=CARTESIAN_POINT('Ctrl Pts',(20.4070574409421,16.8,-0.740817279017836));
#22527=CARTESIAN_POINT('Ctrl Pts',(20.570466834294,-12.,-0.750031355028731));
#22528=CARTESIAN_POINT('Ctrl Pts',(20.570466834294,16.8,-0.750031355028731));
#22529=CARTESIAN_POINT('Ctrl Pts',(20.7773607278973,-12.,-0.785302229564316));
#22530=CARTESIAN_POINT('Ctrl Pts',(20.7773607278973,16.8,-0.785302229564316));
#22531=CARTESIAN_POINT('Ctrl Pts',(20.9870805449298,-12.,-0.859882777793607));
#22532=CARTESIAN_POINT('Ctrl Pts',(20.9870805449298,16.8,-0.859882777793607));
#22533=CARTESIAN_POINT('Ctrl Pts',(21.1998878964781,-12.,-0.985918438087056));
#22534=CARTESIAN_POINT('Ctrl Pts',(21.1998878964781,16.8,-0.985918438087056));
#22535=CARTESIAN_POINT('Ctrl Pts',(21.4160984502468,-12.,-1.16513193018819));
#22536=CARTESIAN_POINT('Ctrl Pts',(21.4160984502468,16.8,-1.16513193018819));
#22537=CARTESIAN_POINT('Ctrl Pts',(21.6360629244597,-12.,-1.38851558520595));
#22538=CARTESIAN_POINT('Ctrl Pts',(21.6360629244597,16.8,-1.38851558520595));
#22539=CARTESIAN_POINT('Ctrl Pts',(21.8601428560791,-12.,-1.64103427806176));
#22540=CARTESIAN_POINT('Ctrl Pts',(21.8601428560791,16.8,-1.64103427806176));
#22541=CARTESIAN_POINT('Ctrl Pts',(22.0886743686473,-12.,-1.90460559759654));
#22542=CARTESIAN_POINT('Ctrl Pts',(22.0886743686473,16.8,-1.90460559759654));
#22543=CARTESIAN_POINT('Ctrl Pts',(22.3219273279567,-12.,-2.16140314464429));
#22544=CARTESIAN_POINT('Ctrl Pts',(22.3219273279567,16.8,-2.16140314464429));
#22545=CARTESIAN_POINT('Ctrl Pts',(22.5600378010161,-12.,-2.3973000769867));
#22546=CARTESIAN_POINT('Ctrl Pts',(22.5600378010161,16.8,-2.3973000769867));
#22547=CARTESIAN_POINT('Ctrl Pts',(22.8029682104327,-12.,-2.60422537589526));
#22548=CARTESIAN_POINT('Ctrl Pts',(22.8029682104327,16.8,-2.60422537589526));
#22549=CARTESIAN_POINT('Ctrl Pts',(23.0506005766976,-12.,-2.77805908652226));
#22550=CARTESIAN_POINT('Ctrl Pts',(23.0506005766976,16.8,-2.77805908652226));
#22551=CARTESIAN_POINT('Ctrl Pts',(23.2523538070279,-12.,-2.88956861747599));
#22552=CARTESIAN_POINT('Ctrl Pts',(23.2523538070279,16.8,-2.88956861747599));
#22553=CARTESIAN_POINT('Ctrl Pts',(23.4056687844597,-12.,-2.95772702235629));
#22554=CARTESIAN_POINT('Ctrl Pts',(23.4056687844597,16.8,-2.95772702235629));
#22555=CARTESIAN_POINT('Ctrl Pts',(23.5087612184661,-12.,-2.99633939947042));
#22556=CARTESIAN_POINT('Ctrl Pts',(23.5087612184661,16.8,-2.99633939947042));
#22557=CARTESIAN_POINT('Ctrl Pts',(23.560528050594,-12.,-3.01393888949139));
#22558=CARTESIAN_POINT('Ctrl Pts',(23.560528050594,16.8,-3.01393888949139));
#22559=CARTESIAN_POINT('',(23.5207683417462,-1.63165946910082,-3.));
#22560=CARTESIAN_POINT('',(23.5207683417462,-1.63165946910082,-3.));
#22561=CARTESIAN_POINT('Ctrl Pts',(20.1650770882888,-1.63165946910082,-0.737782898536615));
#22562=CARTESIAN_POINT('Ctrl Pts',(20.2051790492699,-1.63165946910082,-0.737782898536615));
#22563=CARTESIAN_POINT('Ctrl Pts',(20.2856318058959,-1.63165946910082,-0.738334262610078));
#22564=CARTESIAN_POINT('Ctrl Pts',(20.4070574409421,-1.63165946910082,-0.740817279017836));
#22565=CARTESIAN_POINT('Ctrl Pts',(20.570466834294,-1.63165946910082,-0.750031355028731));
#22566=CARTESIAN_POINT('Ctrl Pts',(20.7773607278973,-1.63165946910082,-0.785302229564316));
#22567=CARTESIAN_POINT('Ctrl Pts',(20.9870805449298,-1.63165946910082,-0.859882777793607));
#22568=CARTESIAN_POINT('Ctrl Pts',(21.1998878964781,-1.63165946910082,-0.985918438087056));
#22569=CARTESIAN_POINT('Ctrl Pts',(21.4160984502468,-1.63165946910082,-1.16513193018819));
#22570=CARTESIAN_POINT('Ctrl Pts',(21.6360629244597,-1.63165946910082,-1.38851558520595));
#22571=CARTESIAN_POINT('Ctrl Pts',(21.8601428560791,-1.63165946910082,-1.64103427806176));
#22572=CARTESIAN_POINT('Ctrl Pts',(22.0886743686473,-1.63165946910082,-1.90460559759654));
#22573=CARTESIAN_POINT('Ctrl Pts',(22.3219273279567,-1.63165946910082,-2.16140314464429));
#22574=CARTESIAN_POINT('Ctrl Pts',(22.5600378010161,-1.63165946910082,-2.3973000769867));
#22575=CARTESIAN_POINT('Ctrl Pts',(22.8029682104327,-1.63165946910082,-2.60422537589526));
#22576=CARTESIAN_POINT('Ctrl Pts',(23.0429827907474,-1.63165946910082,-2.77271153031038));
#22577=CARTESIAN_POINT('Ctrl Pts',(23.2368431253681,-1.63165946910082,-2.88095209536456));
#22578=CARTESIAN_POINT('Ctrl Pts',(23.3821028186481,-1.63165946910082,-2.94712138325619));
#22579=CARTESIAN_POINT('Ctrl Pts',(23.4770787559704,-1.63165946910082,-2.98421892689512));
#22580=CARTESIAN_POINT('Ctrl Pts',(23.5207683417462,-1.63165946910082,-3.));
#22581=CARTESIAN_POINT('Origin',(14.1696121318917,-2.14824178200142,-3.));
#22582=CARTESIAN_POINT('',(25.8992960798277,-1.63165946910082,-3.));
#22583=CARTESIAN_POINT('',(25.8992960798277,0.,-3.));
#22584=CARTESIAN_POINT('',(19.2071026744088,-1.63165946910082,-3.));
#22585=CARTESIAN_POINT('Origin',(24.7143466872546,0.,-0.395297377936459));
#22586=CARTESIAN_POINT('',(27.575916328613,-1.63165946910082,-0.395297377936459));
#22587=CARTESIAN_POINT('',(27.575916328613,0.,-0.395297377936459));
#22588=CARTESIAN_POINT('Origin',(24.7143466872546,-1.63165946910082,-0.395297377936459));
#22589=CARTESIAN_POINT('Origin',(24.7143466872546,0.,5.90470262206354));
#22590=CARTESIAN_POINT('',(21.9988718582129,-1.63165946910082,6.80735275649273));
#22591=CARTESIAN_POINT('',(21.9988718582129,0.,6.80735275649273));
#22592=CARTESIAN_POINT('',(27.575916328613,-1.63165946910082,5.90470262206354));
#22593=CARTESIAN_POINT('Origin',(24.7143466872546,-1.63165946910082,5.90470262206354));
#22594=CARTESIAN_POINT('',(27.575916328613,0.,5.90470262206354));
#22595=CARTESIAN_POINT('Origin',(20.1650770882888,0.,7.59525803303831));
#22596=CARTESIAN_POINT('',(20.1650770882888,-1.63165946910082,5.59936274946018));
#22597=CARTESIAN_POINT('',(20.1650770882888,0.,5.59936274946018));
#22598=CARTESIAN_POINT('Origin',(20.1650770882888,-1.63165946910082,7.59525803303831));
#22599=CARTESIAN_POINT('Origin',(20.1650770882888,0.,5.59936274946018));
#22600=CARTESIAN_POINT('',(5.09382715545311,-4.33051922028271,5.59936274946018));
#22601=CARTESIAN_POINT('Origin',(5.09382715545311,0.,5.59936274946018));
#22602=CARTESIAN_POINT('',(13.9521549326808,-4.33051922028271,5.59936274946018));
#22603=CARTESIAN_POINT('',(12.629452121871,-4.33051922028271,5.59936274946018));
#22604=CARTESIAN_POINT('',(19.2071026744088,-1.63165946910082,5.59936274946018));
#22605=CARTESIAN_POINT('Ctrl Pts',(19.2071026744088,-1.63165946910082,5.59936274946018));
#22606=CARTESIAN_POINT('Ctrl Pts',(19.1308048362197,-1.63165946910082,5.59936274946018));
#22607=CARTESIAN_POINT('Ctrl Pts',(18.9779068684107,-1.63172180635354,5.59936274946018));
#22608=CARTESIAN_POINT('Ctrl Pts',(18.7476534820197,-1.63200385678456,5.59936274946018));
#22609=CARTESIAN_POINT('Ctrl Pts',(18.4399535686149,-1.63662374391445,5.59936274946018));
#22610=CARTESIAN_POINT('Ctrl Pts',(18.0602469444161,-1.6704655276535,5.59936274946018));
#22611=CARTESIAN_POINT('Ctrl Pts',(17.6925082784732,-1.75662630260534,5.59936274946018));
#22612=CARTESIAN_POINT('Ctrl Pts',(17.3426063821155,-1.91508101584403,5.59936274946018));
#22613=CARTESIAN_POINT('Ctrl Pts',(17.0126841408516,-2.15256650575318,5.59936274946018));
#22614=CARTESIAN_POINT('Ctrl Pts',(16.6994685020962,-2.45665970286042,5.59936274946018));
#22615=CARTESIAN_POINT('Ctrl Pts',(16.396392567999,-2.80347808583323,5.59936274946018));
#22616=CARTESIAN_POINT('Ctrl Pts',(16.0950135392462,-3.16285055044176,5.59936274946018));
#22617=CARTESIAN_POINT('Ctrl Pts',(15.7866049591328,-3.50410652905647,5.59936274946018));
#22618=CARTESIAN_POINT('Ctrl Pts',(15.4636185066764,-3.80138932605477,5.59936274946018));
#22619=CARTESIAN_POINT('Ctrl Pts',(15.1212896693278,-4.03949049111154,5.59936274946018));
#22620=CARTESIAN_POINT('Ctrl Pts',(14.7569409494257,-4.21100033264776,5.59936274946018));
#22621=CARTESIAN_POINT('Ctrl Pts',(14.4468469322399,-4.29305314840303,5.59936274946018));
#22622=CARTESIAN_POINT('Ctrl Pts',(14.2036369078635,-4.3237071977066,5.59936274946018));
#22623=CARTESIAN_POINT('Ctrl Pts',(14.0367700658778,-4.33051922028271,5.59936274946018));
#22624=CARTESIAN_POINT('Ctrl Pts',(13.9521549326808,-4.33051922028271,5.59936274946018));
#22625=CARTESIAN_POINT('',(19.6860898813488,-1.63165946910082,5.59936274946018));
#22626=CARTESIAN_POINT('',(5.1457717363639,-2.68051922028271,5.59936274946018));
#22627=CARTESIAN_POINT('',(17.0586160104848,-2.68051922028271,5.59936274946018));
#22628=CARTESIAN_POINT('',(5.1457717363639,-2.6650130345292,5.59936274946018));
#22629=CARTESIAN_POINT('',(5.1457717363639,-1.34025961014136,5.59936274946018));
#22630=CARTESIAN_POINT('Origin',(5.09382715545311,0.,5.59936274946018));
#22631=CARTESIAN_POINT('Origin',(24.7143466872546,0.,5.90470262206354));
#22632=CARTESIAN_POINT('',(23.013011518287,-1.63165946910082,5.90470262206354));
#22633=CARTESIAN_POINT('Origin',(24.7143466872546,-1.63165946910082,5.90470262206354));
#22634=CARTESIAN_POINT('',(23.013011518287,0.,5.90470262206354));
#22635=CARTESIAN_POINT('Origin',(24.7143466872546,0.,-0.395297377936459));
#22636=CARTESIAN_POINT('',(23.013011518287,-1.63165946910082,-0.395297377936459));
#22637=CARTESIAN_POINT('Origin',(24.7143466872546,-1.63165946910082,-0.395297377936459));
#22638=CARTESIAN_POINT('',(23.013011518287,0.,-0.395297377936459));
#22639=CARTESIAN_POINT('Origin',(27.575916328613,-1.63165946910082,0.));
#22640=CARTESIAN_POINT('',(27.575916328613,-1.63165946910082,0.));
#22641=CARTESIAN_POINT('Ctrl Pts',(13.9521549326808,-4.33051922028271,-3.));
#22642=CARTESIAN_POINT('Ctrl Pts',(13.9521549326808,-4.33051922028271,11.4));
#22643=CARTESIAN_POINT('Ctrl Pts',(14.0367700658778,-4.33051922028271,-3.));
#22644=CARTESIAN_POINT('Ctrl Pts',(14.0367700658778,-4.33051922028271,11.4));
#22645=CARTESIAN_POINT('Ctrl Pts',(14.2036369078635,-4.3237071977066,-3.));
#22646=CARTESIAN_POINT('Ctrl Pts',(14.2036369078635,-4.3237071977066,11.4));
#22647=CARTESIAN_POINT('Ctrl Pts',(14.4468469322399,-4.29305314840303,-3.));
#22648=CARTESIAN_POINT('Ctrl Pts',(14.4468469322399,-4.29305314840303,11.4));
#22649=CARTESIAN_POINT('Ctrl Pts',(14.7569409494257,-4.21100033264776,-3.));
#22650=CARTESIAN_POINT('Ctrl Pts',(14.7569409494257,-4.21100033264776,11.4));
#22651=CARTESIAN_POINT('Ctrl Pts',(15.1212896693278,-4.03949049111154,-3.));
#22652=CARTESIAN_POINT('Ctrl Pts',(15.1212896693278,-4.03949049111154,11.4));
#22653=CARTESIAN_POINT('Ctrl Pts',(15.4636185066764,-3.80138932605477,-3.));
#22654=CARTESIAN_POINT('Ctrl Pts',(15.4636185066764,-3.80138932605477,11.4));
#22655=CARTESIAN_POINT('Ctrl Pts',(15.7866049591328,-3.50410652905647,-3.));
#22656=CARTESIAN_POINT('Ctrl Pts',(15.7866049591328,-3.50410652905647,11.4));
#22657=CARTESIAN_POINT('Ctrl Pts',(16.0950135392462,-3.16285055044176,-3.));
#22658=CARTESIAN_POINT('Ctrl Pts',(16.0950135392462,-3.16285055044176,11.4));
#22659=CARTESIAN_POINT('Ctrl Pts',(16.396392567999,-2.80347808583323,-3.));
#22660=CARTESIAN_POINT('Ctrl Pts',(16.396392567999,-2.80347808583323,11.4));
#22661=CARTESIAN_POINT('Ctrl Pts',(16.6994685020962,-2.45665970286042,-3.));
#22662=CARTESIAN_POINT('Ctrl Pts',(16.6994685020962,-2.45665970286042,11.4));
#22663=CARTESIAN_POINT('Ctrl Pts',(17.0126841408516,-2.15256650575318,-3.));
#22664=CARTESIAN_POINT('Ctrl Pts',(17.0126841408516,-2.15256650575318,11.4));
#22665=CARTESIAN_POINT('Ctrl Pts',(17.3426063821155,-1.91508101584403,-3.));
#22666=CARTESIAN_POINT('Ctrl Pts',(17.3426063821155,-1.91508101584403,11.4));
#22667=CARTESIAN_POINT('Ctrl Pts',(17.6925082784732,-1.75662630260534,-3.));
#22668=CARTESIAN_POINT('Ctrl Pts',(17.6925082784732,-1.75662630260534,11.4));
#22669=CARTESIAN_POINT('Ctrl Pts',(18.0602469444161,-1.6704655276535,-3.));
#22670=CARTESIAN_POINT('Ctrl Pts',(18.0602469444161,-1.6704655276535,11.4));
#22671=CARTESIAN_POINT('Ctrl Pts',(18.4399535686149,-1.63662374391445,-3.));
#22672=CARTESIAN_POINT('Ctrl Pts',(18.4399535686149,-1.63662374391445,11.4));
#22673=CARTESIAN_POINT('Ctrl Pts',(18.7476534820197,-1.63200385678456,-3.));
#22674=CARTESIAN_POINT('Ctrl Pts',(18.7476534820197,-1.63200385678456,11.4));
#22675=CARTESIAN_POINT('Ctrl Pts',(18.9779068684107,-1.63172180635354,-3.));
#22676=CARTESIAN_POINT('Ctrl Pts',(18.9779068684107,-1.63172180635354,11.4));
#22677=CARTESIAN_POINT('Ctrl Pts',(19.1308048362197,-1.63165946910082,-3.));
#22678=CARTESIAN_POINT('Ctrl Pts',(19.1308048362197,-1.63165946910082,11.4));
#22679=CARTESIAN_POINT('Ctrl Pts',(19.2071026744088,-1.63165946910082,-3.));
#22680=CARTESIAN_POINT('Ctrl Pts',(19.2071026744088,-1.63165946910082,11.4));
#22681=CARTESIAN_POINT('',(19.2071026744088,-1.63165946910082,0.));
#22682=CARTESIAN_POINT('',(13.9521549326808,-4.33051922028271,0.));
#22683=CARTESIAN_POINT('Origin',(19.2071026744088,-1.63165946910082,0.));
#22684=CARTESIAN_POINT('Origin',(5.09382715545311,-4.33051922028271,0.));
#22685=CARTESIAN_POINT('',(5.09382715545311,-4.33051922028271,0.));
#22686=CARTESIAN_POINT('Origin',(5.09382715545311,0.,0.));
#22687=CARTESIAN_POINT('Origin',(5.09382715545311,0.,0.));
#22688=CARTESIAN_POINT('',(5.1457717363639,-2.6650130345292,0.));
#22689=CARTESIAN_POINT('Origin',(5.1457717363639,-2.68051922028271,0.));
#22690=CARTESIAN_POINT('',(5.1457717363639,-2.68051922028271,0.));
#22691=CARTESIAN_POINT('Origin',(13.9521549326808,-2.68051922028271,0.));
#22692=CARTESIAN_POINT('',(0.,0.,0.));
#22693=CARTESIAN_POINT('Ctrl Pts',(46.6861496741435,4.13165936500604,6.75210248110235));
#22694=CARTESIAN_POINT('Ctrl Pts',(46.6467382040187,4.13173032837167,6.8615039640666));
#22695=CARTESIAN_POINT('Ctrl Pts',(46.5809898678815,4.07139842264618,7.04401340746142));
#22696=CARTESIAN_POINT('Ctrl Pts',(46.5181050726922,3.86354903122596,7.21857400689702));
#22697=CARTESIAN_POINT('Ctrl Pts',(46.5046271380005,3.70887953224881,7.25598712642546));
#22698=CARTESIAN_POINT('Ctrl Pts',(46.5046469694585,3.63131831090395,7.25593207669225));
#22699=CARTESIAN_POINT('Ctrl Pts',(46.6861648307274,4.2064483703636,6.75206052368169));
#22700=CARTESIAN_POINT('Ctrl Pts',(46.6415880227693,4.2102116935304,6.87576092573886));
#22701=CARTESIAN_POINT('Ctrl Pts',(46.5658363543261,4.14848673640705,7.0861290861269));
#22702=CARTESIAN_POINT('Ctrl Pts',(46.4900735883089,3.90919827275704,7.29633200080862));
#22703=CARTESIAN_POINT('Ctrl Pts',(46.4733614735456,3.72414766997645,7.34277691560461));
#22704=CARTESIAN_POINT('Ctrl Pts',(46.4733860630999,3.63125085693363,7.34270857847526));
#22705=CARTESIAN_POINT('Ctrl Pts',(46.7183800447354,4.35575113079639,6.76357123269517));
#22706=CARTESIAN_POINT('Ctrl Pts',(46.6667328898876,4.36685422640062,6.91699804310752));
#22707=CARTESIAN_POINT('Ctrl Pts',(46.5768274780168,4.30231304999428,7.18491601275544));
#22708=CARTESIAN_POINT('Ctrl Pts',(46.4820223126629,4.00023029397859,7.46856355573902));
#22709=CARTESIAN_POINT('Ctrl Pts',(46.4603525972319,3.75460132906098,7.53347058371532));
#22710=CARTESIAN_POINT('Ctrl Pts',(46.460384480148,3.63111631405149,7.53337508531403));
#22711=CARTESIAN_POINT('Ctrl Pts',(46.8757561668702,4.56603451100179,6.82013223242444));
#22712=CARTESIAN_POINT('Ctrl Pts',(46.8243018044365,4.58250926196892,7.01900975145347));
#22713=CARTESIAN_POINT('Ctrl Pts',(46.7343292407208,4.5031002935665,7.36952281620736));
#22714=CARTESIAN_POINT('Ctrl Pts',(46.638383000099,4.1127406122417,7.74468925829955));
#22715=CARTESIAN_POINT('Ctrl Pts',(46.616220839815,3.7921233777235,7.83123568433033));
#22716=CARTESIAN_POINT('Ctrl Pts',(46.6162534469586,3.63095054220852,7.83110834859193));
#22717=CARTESIAN_POINT('Ctrl Pts',(47.0510239491272,4.63163976411415,6.88322984349305));
#22718=CARTESIAN_POINT('Ctrl Pts',(47.0082783943361,4.64056070504751,7.09954757890675));
#22719=CARTESIAN_POINT('Ctrl Pts',(46.9358664296334,4.53765652876905,7.46970543244382));
#22720=CARTESIAN_POINT('Ctrl Pts',(46.8630216802537,4.12014583132121,7.84521978438382));
#22721=CARTESIAN_POINT('Ctrl Pts',(46.8469158520526,3.79451524716846,7.92824101697815));
#22722=CARTESIAN_POINT('Ctrl Pts',(46.8469395494882,3.63093997420058,7.92811886303569));
#22723=CARTESIAN_POINT('Ctrl Pts',(47.1565761357334,4.63165926631602,6.92125495912786));
#22724=CARTESIAN_POINT('Ctrl Pts',(47.1190493074978,4.63179909627843,7.13934266665166));
#22725=CARTESIAN_POINT('Ctrl Pts',(47.0568496727956,4.51113104304455,7.50308186089014));
#22726=CARTESIAN_POINT('Ctrl Pts',(46.9978527681235,4.09543269263203,7.85086983906624));
#22727=CARTESIAN_POINT('Ctrl Pts',(46.985256719747,3.78609758552286,7.92539939233487));
#22728=CARTESIAN_POINT('Ctrl Pts',(46.9852752536658,3.63097716158626,7.92528972939672));
#22729=CARTESIAN_POINT('',(46.4793862705605,3.63165946910083,7.4910739147271));
#22730=CARTESIAN_POINT('',(46.9852421795911,3.63165946910083,7.92529064498531));
#22731=CARTESIAN_POINT('Origin',(46.9750537087877,3.63165946910083,7.42539446070033));
#22732=CARTESIAN_POINT('',(47.1564408307335,4.63165946910083,6.92188570884001));
#22733=CARTESIAN_POINT('Ctrl Pts',(46.9852421795911,3.63165946910083,7.92529064498533));
#22734=CARTESIAN_POINT('Ctrl Pts',(46.9852421795911,3.67152847702579,7.92529064498533));
#22735=CARTESIAN_POINT('Ctrl Pts',(46.9856617576314,3.71139629383976,7.92289294206818));
#22736=CARTESIAN_POINT('Ctrl Pts',(46.9864809263889,3.75094114378544,7.91812438514576));
#22737=CARTESIAN_POINT('Ctrl Pts',(46.987300394655,3.79050045231676,7.91335408471972));
#22738=CARTESIAN_POINT('Ctrl Pts',(46.9885197537897,3.82973593634109,7.90621131868988));
#22739=CARTESIAN_POINT('Ctrl Pts',(46.990120623989,3.86833498313616,7.8967743079273));
#22740=CARTESIAN_POINT('Ctrl Pts',(46.991725286537,3.90702546835329,7.88731494155118));
#22741=CARTESIAN_POINT('Ctrl Pts',(46.9937132815878,3.94507590371365,7.87555067389803));
#22742=CARTESIAN_POINT('Ctrl Pts',(46.9960675879378,3.98219017156174,7.86160926054568));
#22743=CARTESIAN_POINT('Ctrl Pts',(46.9981383536307,4.01483458615883,7.84934687995914));
#22744=CARTESIAN_POINT('Ctrl Pts',(47.0004925394058,4.04675480199022,7.83540106098309));
#22745=CARTESIAN_POINT('Ctrl Pts',(47.0031193862113,4.07776647838611,7.81988733921945));
#22746=CARTESIAN_POINT('Ctrl Pts',(47.0063554421103,4.11597027395028,7.80077572954276));
#22747=CARTESIAN_POINT('Ctrl Pts',(47.0100043369411,4.15281712248742,7.77927345884883));
#22748=CARTESIAN_POINT('Ctrl Pts',(47.0140201692982,4.18802664862582,7.75561393361822));
#22749=CARTESIAN_POINT('Ctrl Pts',(47.0180513055259,4.22337035417768,7.73186424468573));
#22750=CARTESIAN_POINT('Ctrl Pts',(47.0224522066382,4.25706392790331,7.70594127813406));
#22751=CARTESIAN_POINT('Ctrl Pts',(47.0271771428546,4.28886502022712,7.67811395812653));
#22752=CARTESIAN_POINT('Ctrl Pts',(47.0319338280211,4.32087979824855,7.65009965396675));
#22753=CARTESIAN_POINT('Ctrl Pts',(47.0370189428221,4.35097632510684,7.62015580277312));
#22754=CARTESIAN_POINT('Ctrl Pts',(47.0423861535344,4.37895330700274,7.58858295363978));
#22755=CARTESIAN_POINT('Ctrl Pts',(47.0453675812267,4.39449421885468,7.5710445763008));
#22756=CARTESIAN_POINT('Ctrl Pts',(47.0484360582723,4.40938194656237,7.55300396459847));
#22757=CARTESIAN_POINT('Ctrl Pts',(47.051583642697,4.42358842273374,7.53451522576715));
#22758=CARTESIAN_POINT('Ctrl Pts',(47.0581899359112,4.45340562045305,7.49571022059454));
#22759=CARTESIAN_POINT('Ctrl Pts',(47.065142388108,4.48023980475269,7.4549047021496));
#22760=CARTESIAN_POINT('Ctrl Pts',(47.0723688007126,4.50391212229452,7.41254059878685));
#22761=CARTESIAN_POINT('Ctrl Pts',(47.0798141341055,4.52830158161893,7.36889309473683));
#22762=CARTESIAN_POINT('Ctrl Pts',(47.087550305732,4.54933477550803,7.3235912995658));
#22763=CARTESIAN_POINT('Ctrl Pts',(47.095497140004,4.56687155697433,7.27711929567226));
#22764=CARTESIAN_POINT('Ctrl Pts',(47.1035574048721,4.58465865290626,7.22998396511051));
#22765=CARTESIAN_POINT('Ctrl Pts',(47.111834408255,4.59884897342125,7.18164485798867));
#22766=CARTESIAN_POINT('Ctrl Pts',(47.1202429072472,4.60935039329557,7.132606053074));
#22767=CARTESIAN_POINT('Ctrl Pts',(47.1287650304598,4.61999371907335,7.08290458577658));
#22768=CARTESIAN_POINT('Ctrl Pts',(47.1374222396982,4.62684784892612,7.03248439243499));
#22769=CARTESIAN_POINT('Ctrl Pts',(47.1461239307463,4.62987020526441,6.98186857301297));
#22770=CARTESIAN_POINT('Ctrl Pts',(47.1495578751189,4.63106291636878,6.96189407526204));
#22771=CARTESIAN_POINT('Ctrl Pts',(47.1529987256109,4.63165946910083,6.94188909356262));
#22772=CARTESIAN_POINT('Ctrl Pts',(47.1564408307335,4.63165946910083,6.92188570884));
#22773=CARTESIAN_POINT('',(46.686034047791,4.13165946910083,6.7524234458973));
#22774=CARTESIAN_POINT('Origin',(47.1564408307335,4.13165946910083,6.92188570884002));
#22775=CARTESIAN_POINT('',(46.5046469258452,3.63165946910083,7.25593219775761));
#22776=CARTESIAN_POINT('Ctrl Pts',(46.686034047791,4.13165946910083,6.7524234458973));
#22777=CARTESIAN_POINT('Ctrl Pts',(46.6466610234604,4.13165946910083,6.86171820797849));
#22778=CARTESIAN_POINT('Ctrl Pts',(46.5809635080922,4.07131129719481,7.04408657905414));
#22779=CARTESIAN_POINT('Ctrl Pts',(46.5181314324815,3.86363615667733,7.2185008353043));
#22780=CARTESIAN_POINT('Ctrl Pts',(46.5046469258452,3.70910645473421,7.25593219775761));
#22781=CARTESIAN_POINT('Ctrl Pts',(46.5046469258452,3.63165946910083,7.25593219775761));
#22782=CARTESIAN_POINT('Origin',(46.8597130365341,3.63165946910083,7.41851908154457));
#22783=CARTESIAN_POINT('Ctrl Pts',(46.5046473528159,-3.63059149855109,7.25593101253869));
#22784=CARTESIAN_POINT('Ctrl Pts',(46.5045851322103,-3.70839938355921,7.25610372942774));
#22785=CARTESIAN_POINT('Ctrl Pts',(46.5146795236394,-3.82415536695909,7.228082917505));
#22786=CARTESIAN_POINT('Ctrl Pts',(46.5678509837999,-4.04941234271178,7.08048536342935));
#22787=CARTESIAN_POINT('Ctrl Pts',(46.6337785675335,-4.1319627243891,6.89747835034739));
#22788=CARTESIAN_POINT('Ctrl Pts',(46.6863959957155,-4.13165842258026,6.75141872215656));
#22789=CARTESIAN_POINT('Ctrl Pts',(46.4733865349565,-3.6303803307724,7.34270726672911));
#22790=CARTESIAN_POINT('Ctrl Pts',(46.4733098915423,-3.72357375245234,7.34292032668699));
#22791=CARTESIAN_POINT('Ctrl Pts',(46.4857448581586,-3.86198192710135,7.30835231108237));
#22792=CARTESIAN_POINT('Ctrl Pts',(46.5502018222126,-4.12463364349051,7.12951212492674));
#22793=CARTESIAN_POINT('Ctrl Pts',(46.6269356550349,-4.21168567686206,6.91642084451281));
#22794=CARTESIAN_POINT('Ctrl Pts',(46.6864434208004,-4.20642428381315,6.75128743826182));
#22795=CARTESIAN_POINT('Ctrl Pts',(46.4603850872009,-3.62995913755521,7.5333732676333));
#22796=CARTESIAN_POINT('Ctrl Pts',(46.4602864022167,-3.75384045282994,7.53366876770548));
#22797=CARTESIAN_POINT('Ctrl Pts',(46.4762986367123,-3.93741399174525,7.485722011047));
#22798=CARTESIAN_POINT('Ctrl Pts',(46.557549294366,-4.27471561178946,7.24255755482672));
#22799=CARTESIAN_POINT('Ctrl Pts',(46.6497653146017,-4.37079649213517,6.96740001798986));
#22800=CARTESIAN_POINT('Ctrl Pts',(46.7187027995757,-4.35568103713875,6.7626124413514));
#22801=CARTESIAN_POINT('Ctrl Pts',(46.6162653945892,-3.6294401541011,7.8311275649258));
#22802=CARTESIAN_POINT('Ctrl Pts',(46.6161646216497,-3.79113322873311,7.83152127712809));
#22803=CARTESIAN_POINT('Ctrl Pts',(46.6325160222927,-4.03070572037737,7.76763770947141));
#22804=CARTESIAN_POINT('Ctrl Pts',(46.7149034765713,-4.46813006456083,7.44558925601383));
#22805=CARTESIAN_POINT('Ctrl Pts',(46.8074107262328,-4.588317987608,7.08433941933847));
#22806=CARTESIAN_POINT('Ctrl Pts',(46.8760891498065,-4.56594592129301,6.81889353011202));
#22807=CARTESIAN_POINT('Ctrl Pts',(46.8469869465433,-3.62940711399243,7.92813626289466));
#22808=CARTESIAN_POINT('Ctrl Pts',(46.8469132135861,-3.79350638218252,7.92851633731934));
#22809=CARTESIAN_POINT('Ctrl Pts',(46.8588759569925,-4.03697057004181,7.86685151402129));
#22810=CARTESIAN_POINT('Ctrl Pts',(46.9209122979257,-4.49671412053998,7.5470074194169));
#22811=CARTESIAN_POINT('Ctrl Pts',(46.9942655102648,-4.64391672140692,7.17065803186552));
#22812=CARTESIAN_POINT('Ctrl Pts',(47.0513267498103,-4.63159638131279,6.88189077518217));
#22813=CARTESIAN_POINT('Ctrl Pts',(46.9853459842389,-3.62952361504528,7.92528616511393));
#22814=CARTESIAN_POINT('Ctrl Pts',(46.9852878014976,-3.78513304186471,7.92563022056898));
#22815=CARTESIAN_POINT('Ctrl Pts',(46.9947270293396,-4.01663607192479,7.86981222866872));
#22816=CARTESIAN_POINT('Ctrl Pts',(47.0445674957162,-4.46714312456898,7.57576607873376));
#22817=CARTESIAN_POINT('Ctrl Pts',(47.1067651506559,-4.63225727414747,7.21107711520724));
#22818=CARTESIAN_POINT('Ctrl Pts',(47.1568643602425,-4.63165742900804,6.91991124874024));
#22819=CARTESIAN_POINT('',(46.686034047791,-4.13165946910082,6.7524234458973));
#22820=CARTESIAN_POINT('',(47.1564408307335,-4.63165946910082,6.92188570884001));
#22821=CARTESIAN_POINT('Origin',(47.1564408307335,-4.13165946910082,6.92188570884002));
#22822=CARTESIAN_POINT('',(46.9852421795911,-3.63165946910083,7.92529064498531));
#22823=CARTESIAN_POINT('Ctrl Pts',(47.1564408307335,-4.63165946910083,6.92188570884));
#22824=CARTESIAN_POINT('Ctrl Pts',(47.1480140170322,-4.63165946910083,6.97085713488546));
#22825=CARTESIAN_POINT('Ctrl Pts',(47.1395935372251,-4.62808037647553,7.01986113496256));
#22826=CARTESIAN_POINT('Ctrl Pts',(47.131262570954,-4.62093455138398,7.06841459938196));
#22827=CARTESIAN_POINT('Ctrl Pts',(47.1229974613597,-4.613845214373,7.116584246401));
#22828=CARTESIAN_POINT('Ctrl Pts',(47.1148204463948,-4.60324526052124,7.16431030846801));
#22829=CARTESIAN_POINT('Ctrl Pts',(47.1068110838378,-4.58919780885303,7.21111906483794));
#22830=CARTESIAN_POINT('Ctrl Pts',(47.0988591605656,-4.57525109873224,7.25759213138594));
#22831=CARTESIAN_POINT('Ctrl Pts',(47.0910724786717,-4.5579060519702,7.30316082472435));
#22832=CARTESIAN_POINT('Ctrl Pts',(47.0835274294847,-4.53727617799087,7.34736195753565));
#22833=CARTESIAN_POINT('Ctrl Pts',(47.0761627505453,-4.51713947713545,7.39050642801491));
#22834=CARTESIAN_POINT('Ctrl Pts',(47.0690282667772,-4.49387313010114,7.43234773661696));
#22835=CARTESIAN_POINT('Ctrl Pts',(47.0621939029827,-4.46763272108791,7.4724583193628));
#22836=CARTESIAN_POINT('Ctrl Pts',(47.0551084659439,-4.4404283211574,7.51404244001858));
#22837=CARTESIAN_POINT('Ctrl Pts',(47.0483455830168,-4.41002672598321,7.55376596857338));
#22838=CARTESIAN_POINT('Ctrl Pts',(47.0419822780536,-4.37666097695831,7.59116030088757));
#22839=CARTESIAN_POINT('Ctrl Pts',(47.0360532053804,-4.34557210853064,7.62600284185342));
#22840=CARTESIAN_POINT('Ctrl Pts',(47.0304710043537,-4.31191022757954,7.65882301129956));
#22841=CARTESIAN_POINT('Ctrl Pts',(47.0252976393728,-4.27591443953535,7.68925240584234));
#22842=CARTESIAN_POINT('Ctrl Pts',(47.0249187534582,-4.27327818689815,7.69148098801738));
#22843=CARTESIAN_POINT('Ctrl Pts',(47.0245420604123,-4.27062943822396,7.69369675255096));
#22844=CARTESIAN_POINT('Ctrl Pts',(47.0241675845705,-4.26796829819623,7.69589955768561));
#22845=CARTESIAN_POINT('Ctrl Pts',(47.0200852466292,-4.23895795442667,7.71991337640538));
#22846=CARTESIAN_POINT('Ctrl Pts',(47.0162689643525,-4.20842353959352,7.74242325255637));
#22847=CARTESIAN_POINT('Ctrl Pts',(47.0127500788317,-4.17657725649026,7.76319358679969));
#22848=CARTESIAN_POINT('Ctrl Pts',(47.0092311933109,-4.144730973387,7.783963921043));
#22849=CARTESIAN_POINT('Ctrl Pts',(47.0060096815111,-4.11157336723279,7.8029941292581));
#22850=CARTESIAN_POINT('Ctrl Pts',(47.0031177369572,-4.07735827430611,7.82009076834584));
#22851=CARTESIAN_POINT('Ctrl Pts',(46.9998935700605,-4.03921260175829,7.83915144422086));
#22852=CARTESIAN_POINT('Ctrl Pts',(46.9970796175557,-3.99976085751644,7.85580659935101));
#22853=CARTESIAN_POINT('Ctrl Pts',(46.9946965256702,-3.95932346117812,7.86988171412677));
#22854=CARTESIAN_POINT('Ctrl Pts',(46.9923191156137,-3.91898247672032,7.88392327065184));
#22855=CARTESIAN_POINT('Ctrl Pts',(46.990370497899,-3.8776609874032,7.8953968044727));
#22856=CARTESIAN_POINT('Ctrl Pts',(46.9888726507954,-3.83570196062553,7.90417444862372));
#22857=CARTESIAN_POINT('Ctrl Pts',(46.9873788593879,-3.79385654561952,7.91292832569099));
#22858=CARTESIAN_POINT('Ctrl Pts',(46.9863333881254,-3.75137753185371,7.91900070201506));
#22859=CARTESIAN_POINT('Ctrl Pts',(46.9857597266497,-3.70862276753427,7.92231341004287));
#22860=CARTESIAN_POINT('Ctrl Pts',(46.9854164778235,-3.6830405674236,7.9242955601266));
#22861=CARTESIAN_POINT('Ctrl Pts',(46.9852421795911,-3.6573599489112,7.92529064498533));
#22862=CARTESIAN_POINT('Ctrl Pts',(46.9852421795911,-3.63165946910083,7.92529064498533));
#22863=CARTESIAN_POINT('',(46.4793862705605,-3.63165946910083,7.49107391472711));
#22864=CARTESIAN_POINT('Origin',(46.9750537087877,-3.63165946910083,7.42539446070033));
#22865=CARTESIAN_POINT('',(46.5046469258452,-3.63165946910083,7.25593219775761));
#22866=CARTESIAN_POINT('Origin',(46.8597130365341,-3.63165946910083,7.41851908154457));
#22867=CARTESIAN_POINT('Ctrl Pts',(46.5046469258452,-3.63165946910083,7.25593219775761));
#22868=CARTESIAN_POINT('Ctrl Pts',(46.5046469258452,-3.70910645473421,7.25593219775761));
#22869=CARTESIAN_POINT('Ctrl Pts',(46.5147491688035,-3.82445041356865,7.22788959093758));
#22870=CARTESIAN_POINT('Ctrl Pts',(46.5677813386358,-4.04911729610222,7.08067868999677));
#22871=CARTESIAN_POINT('Ctrl Pts',(46.6335366820169,-4.13165946910083,6.89814979533889));
#22872=CARTESIAN_POINT('Ctrl Pts',(46.686034047791,-4.13165946910082,6.7524234458973));
#22873=CARTESIAN_POINT('Origin',(47.6576678782476,-4.13165946910082,5.53053993751283));
#22874=CARTESIAN_POINT('',(48.4890896340131,-4.13165946910082,1.74735881939682));
#22875=CARTESIAN_POINT('',(48.9594964169556,-4.63165946910082,1.91682108233953));
#22876=CARTESIAN_POINT('Origin',(48.9594964169556,-4.13165946910082,1.91682108233953));
#22877=CARTESIAN_POINT('',(47.6576678782476,-4.63165946910082,5.53053993751283));
#22878=CARTESIAN_POINT('',(47.187261095305,-4.13165946910082,5.36107767457011));
#22879=CARTESIAN_POINT('Ctrl Pts',(48.4890896340131,-4.13165946910082,1.74735881939682));
#22880=CARTESIAN_POINT('Ctrl Pts',(48.528033400252,-4.13165946910082,1.63925562595442));
#22881=CARTESIAN_POINT('Ctrl Pts',(48.59296896781,-4.0698690772923,1.45900233001064));
#22882=CARTESIAN_POINT('Ctrl Pts',(48.6538411747882,-3.86114173341796,1.29002843247154));
#22883=CARTESIAN_POINT('Ctrl Pts',(48.6666566035268,-3.70826210137736,1.25445434948526));
#22884=CARTESIAN_POINT('Ctrl Pts',(48.6666566035268,-3.63165946910083,1.25445434948526));
#22885=CARTESIAN_POINT('Ctrl Pts',(48.4890896340131,-4.2625591630004,1.74735881939682));
#22886=CARTESIAN_POINT('Ctrl Pts',(48.5374817032876,-4.25698138037902,1.61355961347516));
#22887=CARTESIAN_POINT('Ctrl Pts',(48.6157021694607,-4.17210624395573,1.39606123956507));
#22888=CARTESIAN_POINT('Ctrl Pts',(48.6877387227602,-3.91206590758877,1.19649815595369));
#22889=CARTESIAN_POINT('Ctrl Pts',(48.7025708074101,-3.72526406128552,1.1547608553863));
#22890=CARTESIAN_POINT('Ctrl Pts',(48.7025708074101,-3.63165946910083,1.1547608553863));
#22891=CARTESIAN_POINT('Ctrl Pts',(48.5910979765086,-4.52323379775168,1.78410693865264));
#22892=CARTESIAN_POINT('Ctrl Pts',(48.6485962811641,-4.50700223220463,1.59589909277704));
#22893=CARTESIAN_POINT('Ctrl Pts',(48.7401801263016,-4.37605369011658,1.29919670157222));
#22894=CARTESIAN_POINT('Ctrl Pts',(48.8226835402575,-4.01396661770324,1.03419011377791));
#22895=CARTESIAN_POINT('Ctrl Pts',(48.8399066101512,-3.75914369554963,0.97936619857827));
#22896=CARTESIAN_POINT('Ctrl Pts',(48.8399066101512,-3.63165946910082,0.97936619857827));
#22897=CARTESIAN_POINT('Ctrl Pts',(48.8363442091647,-4.63165946910083,1.87245596564607));
#22898=CARTESIAN_POINT('Ctrl Pts',(48.8847421900004,-4.62278702779619,1.65657705029431));
#22899=CARTESIAN_POINT('Ctrl Pts',(48.9644640517391,-4.48805314820043,1.30657194968926));
#22900=CARTESIAN_POINT('Ctrl Pts',(49.03889631391,-4.07555797544749,0.986222066672633));
#22901=CARTESIAN_POINT('Ctrl Pts',(49.0544843934583,-3.77992147471384,0.919526552336082));
#22902=CARTESIAN_POINT('Ctrl Pts',(49.0544843934583,-3.63165946910083,0.919526552336082));
#22903=CARTESIAN_POINT('Ctrl Pts',(48.9594964169557,-4.63165946910083,1.91682108233953));
#22904=CARTESIAN_POINT('Ctrl Pts',(49.002637914566,-4.63165946910083,1.69928191144716));
#22905=CARTESIAN_POINT('Ctrl Pts',(49.0757300098058,-4.50807868548377,1.33641576134982));
#22906=CARTESIAN_POINT('Ctrl Pts',(49.1455292082179,-4.09062399773509,0.996113990481237));
#22907=CARTESIAN_POINT('Ctrl Pts',(49.160334755135,-3.78486473365389,0.924458462629198));
#22908=CARTESIAN_POINT('Ctrl Pts',(49.160334755135,-3.63165946910083,0.924458462629198));
#22909=CARTESIAN_POINT('',(48.6666566035268,-3.63165946910083,1.25445434948526));
#22910=CARTESIAN_POINT('',(49.160334755135,-3.63165946910083,0.924458462629196));
#22911=CARTESIAN_POINT('Origin',(49.1370633864694,-3.63165946910083,1.42391661242798));
#22912=CARTESIAN_POINT('Ctrl Pts',(49.160334755135,-3.63165946910083,0.924458462629198));
#22913=CARTESIAN_POINT('Ctrl Pts',(49.160334755135,-3.78486473365389,0.924458462629198));
#22914=CARTESIAN_POINT('Ctrl Pts',(49.1455292082179,-4.09062399773509,0.996113990481237));
#22915=CARTESIAN_POINT('Ctrl Pts',(49.0757300098058,-4.50807868548377,1.33641576134982));
#22916=CARTESIAN_POINT('Ctrl Pts',(49.002637914566,-4.63165946910083,1.69928191144716));
#22917=CARTESIAN_POINT('Ctrl Pts',(48.9594964169557,-4.63165946910083,1.91682108233953));
#22918=CARTESIAN_POINT('Ctrl Pts',(48.4890896340131,-4.13165946910082,1.74735881939682));
#22919=CARTESIAN_POINT('Ctrl Pts',(48.528033400252,-4.13165946910082,1.63925562595442));
#22920=CARTESIAN_POINT('Ctrl Pts',(48.59296896781,-4.0698690772923,1.45900233001064));
#22921=CARTESIAN_POINT('Ctrl Pts',(48.6538411747882,-3.86114173341796,1.29002843247154));
#22922=CARTESIAN_POINT('Ctrl Pts',(48.6666566035268,-3.70826210137736,1.25445434948526));
#22923=CARTESIAN_POINT('Ctrl Pts',(48.6666566035268,-3.63165946910083,1.25445434948526));
#22924=CARTESIAN_POINT('Origin',(49.1370633864693,-3.63165946910082,1.42391661242798));
#22925=CARTESIAN_POINT('',(48.6666566035268,3.63165946910083,1.25445434948527));
#22926=CARTESIAN_POINT('',(49.160334755135,3.63165946910083,0.924458462629187));
#22927=CARTESIAN_POINT('Origin',(49.1370633864693,3.63165946910083,1.42391661242798));
#22928=CARTESIAN_POINT('',(49.160334755135,-3.63165946910082,0.924458462629194));
#22929=CARTESIAN_POINT('',(48.6666566035268,-3.63165946910082,1.25445434948527));
#22930=CARTESIAN_POINT('Ctrl Pts',(48.6666566035268,3.63165946910083,1.25445434948526));
#22931=CARTESIAN_POINT('Ctrl Pts',(48.6666566035268,3.74656496246816,1.25445434948526));
#22932=CARTESIAN_POINT('Ctrl Pts',(48.6319493120662,4.01324141425168,1.35079760040805));
#22933=CARTESIAN_POINT('Ctrl Pts',(48.541015353828,4.13165946910083,1.60321929012389));
#22934=CARTESIAN_POINT('Ctrl Pts',(48.4890896340131,4.13165946910083,1.74735881939682));
#22935=CARTESIAN_POINT('Ctrl Pts',(48.7025708074101,3.63165946910083,1.1547608553863));
#22936=CARTESIAN_POINT('Ctrl Pts',(48.7025708074101,3.77206824523273,1.1547608553863));
#22937=CARTESIAN_POINT('Ctrl Pts',(48.6621924573285,4.09794567280866,1.26724630381089));
#22938=CARTESIAN_POINT('Ctrl Pts',(48.553613260593,4.25512201950971,1.56895747948715));
#22939=CARTESIAN_POINT('Ctrl Pts',(48.4890896340131,4.2625591630004,1.74735881939682));
#22940=CARTESIAN_POINT('Ctrl Pts',(48.8399066101513,3.63165946910083,0.97936619857827));
#22941=CARTESIAN_POINT('Ctrl Pts',(48.8399066101513,3.82288837992692,0.97936619857827));
#22942=CARTESIAN_POINT('Ctrl Pts',(48.7937718458663,4.26716280005947,1.12633645189498));
#22943=CARTESIAN_POINT('Ctrl Pts',(48.6677634135149,4.50159141936477,1.53315977006196));
#22944=CARTESIAN_POINT('Ctrl Pts',(48.5910979765086,4.52323379775167,1.78410693865264));
#22945=CARTESIAN_POINT('Ctrl Pts',(49.0544843934583,3.63165946910083,0.919526552336082));
#22946=CARTESIAN_POINT('Ctrl Pts',(49.0544843934583,3.85405546772779,0.919526552336082));
#22947=CARTESIAN_POINT('Ctrl Pts',(49.0121746951936,4.37009596294779,1.09945552465902));
#22948=CARTESIAN_POINT('Ctrl Pts',(48.9008757179322,4.61982938830091,1.58461354168167));
#22949=CARTESIAN_POINT('Ctrl Pts',(48.8363442091647,4.63165946910082,1.87245596564607));
#22950=CARTESIAN_POINT('Ctrl Pts',(49.160334755135,3.63165946910083,0.924458462629198));
#22951=CARTESIAN_POINT('Ctrl Pts',(49.160334755135,3.86147045583549,0.924458462629198));
#22952=CARTESIAN_POINT('Ctrl Pts',(49.1200596047313,4.39482335940253,1.11853852679163));
#22953=CARTESIAN_POINT('Ctrl Pts',(49.0170191871873,4.63165946910082,1.6267649545568));
#22954=CARTESIAN_POINT('Ctrl Pts',(48.9594964169557,4.63165946910082,1.91682108233953));
#22955=CARTESIAN_POINT('',(48.4890896340131,4.13165946910083,1.74735881939682));
#22956=CARTESIAN_POINT('',(48.9594964169557,4.63165946910083,1.91682108233953));
#22957=CARTESIAN_POINT('Origin',(48.9594964169557,4.13165946910083,1.91682108233953));
#22958=CARTESIAN_POINT('Ctrl Pts',(48.9594964169557,4.63165946910082,1.91682108233953));
#22959=CARTESIAN_POINT('Ctrl Pts',(49.0170191871873,4.63165946910082,1.6267649545568));
#22960=CARTESIAN_POINT('Ctrl Pts',(49.1200596047313,4.39482335940253,1.11853852679163));
#22961=CARTESIAN_POINT('Ctrl Pts',(49.160334755135,3.86147045583549,0.924458462629198));
#22962=CARTESIAN_POINT('Ctrl Pts',(49.160334755135,3.63165946910083,0.924458462629198));
#22963=CARTESIAN_POINT('Ctrl Pts',(48.6666566035268,3.63165946910083,1.25445434948526));
#22964=CARTESIAN_POINT('Ctrl Pts',(48.6666566035268,3.74656496246816,1.25445434948526));
#22965=CARTESIAN_POINT('Ctrl Pts',(48.6319493120662,4.01324141425168,1.35079760040805));
#22966=CARTESIAN_POINT('Ctrl Pts',(48.541015353828,4.13165946910083,1.60321929012389));
#22967=CARTESIAN_POINT('Ctrl Pts',(48.4890896340131,4.13165946910083,1.74735881939682));
#22968=CARTESIAN_POINT('Origin',(47.6576678782476,4.13165946910082,5.53053993751283));
#22969=CARTESIAN_POINT('',(47.187261095305,4.13165946910082,5.36107767457011));
#22970=CARTESIAN_POINT('',(47.6576678782476,4.63165946910082,5.53053993751283));
#22971=CARTESIAN_POINT('Origin',(46.9750537087877,-3.63165946910082,7.42539446070032));
#22972=CARTESIAN_POINT('',(46.4793852260815,-3.63165946910082,7.49106603180771));
#22973=CARTESIAN_POINT('',(46.9852421795911,-3.63165946910082,7.92529064498532));
#22974=CARTESIAN_POINT('Origin',(57.5530637513316,4.63165946910082,6.17670144644389));
#22975=CARTESIAN_POINT('',(67.849510736113,4.63165946910082,10.0458771867885));
#22976=CARTESIAN_POINT('Origin',(48.2463073637984,4.63165946910082,69.7993133400951));
#22977=CARTESIAN_POINT('',(67.8495107361129,4.63165946910082,9.29710969756502));
#22978=CARTESIAN_POINT('',(67.8495107361129,4.63165946910082,7.38584475819711));
#22979=CARTESIAN_POINT('',(59.746010728986,4.63165946910082,5.83920248277193));
#22980=CARTESIAN_POINT('Ctrl Pts',(59.746010728986,4.63165946910082,5.83920248277193));
#22981=CARTESIAN_POINT('Ctrl Pts',(59.7553520150816,4.63165946910082,5.84546856158671));
#22982=CARTESIAN_POINT('Ctrl Pts',(59.7646938885029,4.63165946910082,5.85173542775135));
#22983=CARTESIAN_POINT('Ctrl Pts',(60.2628303227855,4.63165946910084,6.1858477117844));
#22984=CARTESIAN_POINT('Ctrl Pts',(61.2531647920567,4.63165946910082,6.82066652204582));
#22985=CARTESIAN_POINT('Ctrl Pts',(62.8100479900584,4.63165946910083,7.66426081171851));
#22986=CARTESIAN_POINT('Ctrl Pts',(64.4774359515706,4.63165946910083,8.25725916914412));
#22987=CARTESIAN_POINT('Ctrl Pts',(66.1709303349025,4.63165946910083,8.74915286435064));
#22988=CARTESIAN_POINT('Ctrl Pts',(67.2933262825326,4.63165946910082,9.10437306478713));
#22989=CARTESIAN_POINT('Ctrl Pts',(67.8495107361129,4.63165946910082,9.29710969756502));
#22990=CARTESIAN_POINT('Origin',(48.2394105756736,4.63165946910082,20.6896511931003));
#22991=CARTESIAN_POINT('Origin',(48.2463073637984,3.63165946910083,69.7993133400951));
#22992=CARTESIAN_POINT('',(67.5377890263469,3.63165946910083,10.9960506318292));
#22993=CARTESIAN_POINT('Origin',(48.2463073637984,3.63165946910083,69.7993133400951));
#22994=CARTESIAN_POINT('Origin',(67.849510736113,3.63165946910083,10.0458771867885));
#22995=CARTESIAN_POINT('Origin',(48.2463073637984,-3.63165946910082,69.7993133400951));
#22996=CARTESIAN_POINT('',(67.5377890263469,-3.63165946910083,10.9960506318292));
#22997=CARTESIAN_POINT('Origin',(48.2463073637984,-3.63165946910083,69.7993133400951));
#22998=CARTESIAN_POINT('',(67.5377890263469,-3.63165946910082,10.9960506318292));
#22999=CARTESIAN_POINT('Origin',(48.2463073637984,-3.63165946910083,69.7993133400951));
#23000=CARTESIAN_POINT('',(67.849510736113,-4.63165946910082,10.0458771867885));
#23001=CARTESIAN_POINT('Origin',(48.2463073637984,-4.63165946910082,69.7993133400951));
#23002=CARTESIAN_POINT('Origin',(67.849510736113,-3.63165946910083,10.0458771867885));
#23003=CARTESIAN_POINT('Origin',(46.2566167665501,-3.63165946910082,7.94443397556152));
#23004=CARTESIAN_POINT('',(48.6333391993365,-3.63165946910082,1.34693944114521));
#23005=CARTESIAN_POINT('',(46.2566167665501,-3.63165946910082,7.94443397556152));
#23006=CARTESIAN_POINT('',(48.6333391993365,3.63165946910082,1.3469394411452));
#23007=CARTESIAN_POINT('',(48.6333391993365,-3.63165946910082,1.34693944114521));
#23008=CARTESIAN_POINT('',(46.2566167665501,3.63165946910082,7.94443397556152));
#23009=CARTESIAN_POINT('Ctrl Pts',(60.3030816362698,-3.63165946910082,5.00873755018416));
#23010=CARTESIAN_POINT('Ctrl Pts',(60.3124229223654,-3.63165946910082,5.01500362899892));
#23011=CARTESIAN_POINT('Ctrl Pts',(60.321764208461,-3.63165946910082,5.02126970781368));
#23012=CARTESIAN_POINT('Ctrl Pts',(61.0123101391572,-3.63165946910083,5.48448378590278));
#23013=CARTESIAN_POINT('Ctrl Pts',(62.0505895544972,-3.63165946910083,6.1424866608486));
#23014=CARTESIAN_POINT('Ctrl Pts',(63.4401214267519,-3.63165946910083,6.82140499056667));
#23015=CARTESIAN_POINT('Ctrl Pts',(64.5424665843927,-3.63165946910083,7.2182002185439));
#23016=CARTESIAN_POINT('Ctrl Pts',(65.7313524768425,-3.63165946910082,7.5802308563465));
#23017=CARTESIAN_POINT('Ctrl Pts',(66.9461333967787,-3.63165946910083,7.94539057682941));
#23018=CARTESIAN_POINT('Ctrl Pts',(67.7662134721537,-3.63165946910083,8.20990343773874));
#23019=CARTESIAN_POINT('Ctrl Pts',(68.1769417551788,-3.63165946910083,8.35223461177142));
#23020=CARTESIAN_POINT('Ctrl Pts',(60.3030816362698,-3.93085876944271,5.00873755018416));
#23021=CARTESIAN_POINT('Ctrl Pts',(60.3124229223654,-3.93085876944271,5.01500362899892));
#23022=CARTESIAN_POINT('Ctrl Pts',(60.321764208461,-3.93085876944271,5.02126970781368));
#23023=CARTESIAN_POINT('Ctrl Pts',(61.0123101391572,-3.93085876944271,5.48448378590278));
#23024=CARTESIAN_POINT('Ctrl Pts',(62.0505895544972,-3.93085876944271,6.1424866608486));
#23025=CARTESIAN_POINT('Ctrl Pts',(63.4401214267519,-3.93085876944271,6.82140499056667));
#23026=CARTESIAN_POINT('Ctrl Pts',(64.5424665843927,-3.93085876944271,7.2182002185439));
#23027=CARTESIAN_POINT('Ctrl Pts',(65.7313524768425,-3.93085876944271,7.5802308563465));
#23028=CARTESIAN_POINT('Ctrl Pts',(66.9461333967787,-3.93085876944271,7.94539057682941));
#23029=CARTESIAN_POINT('Ctrl Pts',(67.7662134721537,-3.93085876944271,8.20990343773874));
#23030=CARTESIAN_POINT('Ctrl Pts',(68.1769417551788,-3.93085876944271,8.35223461177142));
#23031=CARTESIAN_POINT('Ctrl Pts',(60.1631225847142,-4.4487252310069,5.21738438992301));
#23032=CARTESIAN_POINT('Ctrl Pts',(60.1724638708098,-4.4487252310069,5.22365046873777));
#23033=CARTESIAN_POINT('Ctrl Pts',(60.1818051569054,-4.4487252310069,5.22991654755253));
#23034=CARTESIAN_POINT('Ctrl Pts',(60.8753903965548,-4.4487252310069,5.69574246490634));
#23035=CARTESIAN_POINT('Ctrl Pts',(61.9223125625907,-4.4487252310069,6.35927401084995));
#23036=CARTESIAN_POINT('Ctrl Pts',(63.3416742095466,-4.4487252310069,7.05326112586659));
#23037=CARTESIAN_POINT('Ctrl Pts',(64.4659491723573,-4.4487252310069,7.45759442605238));
#23038=CARTESIAN_POINT('Ctrl Pts',(65.659435332871,-4.4487252310069,7.82096212027916));
#23039=CARTESIAN_POINT('Ctrl Pts',(66.8721227951014,-4.4487252310069,8.18550871975537));
#23040=CARTESIAN_POINT('Ctrl Pts',(67.6874485389554,-4.4487252310069,8.44852840504606));
#23041=CARTESIAN_POINT('Ctrl Pts',(68.0946776586685,-4.4487252310069,8.58962597275722));
#23042=CARTESIAN_POINT('Ctrl Pts',(59.8710171482611,-4.63165946910083,5.65284658768043));
#23043=CARTESIAN_POINT('Ctrl Pts',(59.8803584343568,-4.63165946910083,5.65911266649519));
#23044=CARTESIAN_POINT('Ctrl Pts',(59.8896997204524,-4.63165946910083,5.66537874530994));
#23045=CARTESIAN_POINT('Ctrl Pts',(60.5926792328869,-4.63165946910082,6.13732137267113));
#23046=CARTESIAN_POINT('Ctrl Pts',(61.6535679847968,-4.63165946910083,6.8114233514931));
#23047=CARTESIAN_POINT('Ctrl Pts',(63.1376324390272,-4.63165946910083,7.53756089343684));
#23048=CARTESIAN_POINT('Ctrl Pts',(64.3069826525201,-4.63165946910083,7.95751277860056));
#23049=CARTESIAN_POINT('Ctrl Pts',(65.509415627788,-4.63165946910082,8.32333666532113));
#23050=CARTESIAN_POINT('Ctrl Pts',(66.7179599089468,-4.63165946910083,8.68677615470624));
#23051=CARTESIAN_POINT('Ctrl Pts',(67.5227731148609,-4.63165946910083,8.94640720339014));
#23052=CARTESIAN_POINT('Ctrl Pts',(67.9229860849654,-4.63165946910083,9.08508022412708));
#23053=CARTESIAN_POINT('Ctrl Pts',(59.7460107289861,-4.63165946910083,5.83920248277199));
#23054=CARTESIAN_POINT('Ctrl Pts',(59.7553520150817,-4.63165946910083,5.84546856158675));
#23055=CARTESIAN_POINT('Ctrl Pts',(59.7646933011773,-4.63165946910083,5.8517346404015));
#23056=CARTESIAN_POINT('Ctrl Pts',(60.4723758535947,-4.63165946910082,6.32644386179577));
#23057=CARTESIAN_POINT('Ctrl Pts',(61.5383304632888,-4.63165946910083,7.00485275615749));
#23058=CARTESIAN_POINT('Ctrl Pts',(63.0506317795768,-4.63165946910083,7.74490586716288));
#23059=CARTESIAN_POINT('Ctrl Pts',(64.2391166337755,-4.63165946910083,8.17151621821202));
#23060=CARTESIAN_POINT('Ctrl Pts',(65.4452319728652,-4.63165946910082,8.53831640988129));
#23061=CARTESIAN_POINT('Ctrl Pts',(66.6520537625864,-4.63165946910083,8.90132071934848));
#23062=CARTESIAN_POINT('Ctrl Pts',(67.4522361264021,-4.63165946910083,9.15944067414874));
#23063=CARTESIAN_POINT('Ctrl Pts',(67.8495107361018,-4.63165946910083,9.29710969756116));
#23064=CARTESIAN_POINT('',(60.331105491743,-3.63165946910083,5.02753578421065));
#23065=CARTESIAN_POINT('',(68.1769417551846,-3.63165946910083,8.35223461177341));
#23066=CARTESIAN_POINT('Ctrl Pts',(60.3311054949517,-3.63165946910082,5.0275357859514));
#23067=CARTESIAN_POINT('Ctrl Pts',(61.0124633196254,-3.63165946910083,5.48458086221223));
#23068=CARTESIAN_POINT('Ctrl Pts',(62.0506664301593,-3.63165946910083,6.14252422191301));
#23069=CARTESIAN_POINT('Ctrl Pts',(63.4401214267519,-3.63165946910083,6.82140499056667));
#23070=CARTESIAN_POINT('Ctrl Pts',(64.5424665843927,-3.63165946910083,7.2182002185439));
#23071=CARTESIAN_POINT('Ctrl Pts',(65.7313524768425,-3.63165946910082,7.5802308563465));
#23072=CARTESIAN_POINT('Ctrl Pts',(66.9461333967787,-3.63165946910083,7.94539057682941));
#23073=CARTESIAN_POINT('Ctrl Pts',(67.7662134721537,-3.63165946910083,8.20990343773874));
#23074=CARTESIAN_POINT('Ctrl Pts',(68.1769417551788,-3.63165946910083,8.35223461177142));
#23075=CARTESIAN_POINT('',(67.8495107361074,-4.63165946910082,9.29710969756116));
#23076=CARTESIAN_POINT('Origin',(67.8495107361018,-3.63165946910083,9.29710969756116));
#23077=CARTESIAN_POINT('',(59.7460107289861,-4.63165946910082,5.839202482772));
#23078=CARTESIAN_POINT('Ctrl Pts',(67.8495107361018,-4.63165946910083,9.29710969756116));
#23079=CARTESIAN_POINT('Ctrl Pts',(67.4522361264021,-4.63165946910083,9.15944067414874));
#23080=CARTESIAN_POINT('Ctrl Pts',(66.6520537625864,-4.63165946910083,8.90132071934848));
#23081=CARTESIAN_POINT('Ctrl Pts',(65.4452319728652,-4.63165946910082,8.53831640988129));
#23082=CARTESIAN_POINT('Ctrl Pts',(64.2391166337755,-4.63165946910083,8.17151621821202));
#23083=CARTESIAN_POINT('Ctrl Pts',(63.0506317795768,-4.63165946910083,7.74490586716288));
#23084=CARTESIAN_POINT('Ctrl Pts',(61.5383304632888,-4.63165946910083,7.00485275615749));
#23085=CARTESIAN_POINT('Ctrl Pts',(60.4723758535947,-4.63165946910082,6.32644386179577));
#23086=CARTESIAN_POINT('Ctrl Pts',(59.7646933011773,-4.63165946910083,5.8517346404015));
#23087=CARTESIAN_POINT('Ctrl Pts',(59.7553520150817,-4.63165946910083,5.84546856158675));
#23088=CARTESIAN_POINT('Ctrl Pts',(59.7460107289861,-4.63165946910083,5.83920248277199));
#23089=CARTESIAN_POINT('Ctrl Pts',(59.7460107289858,-4.63165946910083,5.83920248277159));
#23090=CARTESIAN_POINT('Ctrl Pts',(59.747983173405,-4.63165946910083,5.83760826569162));
#23091=CARTESIAN_POINT('Ctrl Pts',(59.7499465217352,-4.63165033057513,5.83600301592175));
#23092=CARTESIAN_POINT('Ctrl Pts',(59.8106476612128,-4.63108042779695,5.78580377952516));
#23093=CARTESIAN_POINT('Ctrl Pts',(59.8590970533301,-4.62230091506807,5.72906894083519));
#23094=CARTESIAN_POINT('Ctrl Pts',(59.9430417049605,-4.58749976286397,5.60825635642181));
#23095=CARTESIAN_POINT('Ctrl Pts',(59.9774595309507,-4.56225920236549,5.5461849400014));
#23096=CARTESIAN_POINT('Ctrl Pts',(60.0682261303521,-4.47320022945349,5.38630772232757));
#23097=CARTESIAN_POINT('Ctrl Pts',(60.1201210869269,-4.40574630265719,5.31924893308168));
#23098=CARTESIAN_POINT('Ctrl Pts',(60.2084830922883,-4.28319035536618,5.2327413196381));
#23099=CARTESIAN_POINT('Ctrl Pts',(60.27223114969,-4.1877452714611,5.17557566103711));
#23100=CARTESIAN_POINT('Ctrl Pts',(60.320208223554,-3.97475788580983,5.09249114125403));
#23101=CARTESIAN_POINT('Ctrl Pts',(60.3271981253549,-3.90791218641454,5.07054001100713));
#23102=CARTESIAN_POINT('Ctrl Pts',(60.3327487578869,-3.76969211347434,5.03759836393143));
#23103=CARTESIAN_POINT('Ctrl Pts',(60.3311054852527,-3.69976109960378,5.02753577944549));
#23104=CARTESIAN_POINT('Ctrl Pts',(60.3311054852527,-3.63165946910083,5.02753577944548));
#23105=CARTESIAN_POINT('Origin',(67.8495107361129,-3.63165946910083,9.29710969756502));
#23106=CARTESIAN_POINT('',(68.849510736113,-3.63165946910083,9.29710969756497));
#23107=CARTESIAN_POINT('Origin',(67.8495107361129,-3.63165946910083,9.29710969756502));
#23108=CARTESIAN_POINT('Origin',(67.849510736113,-3.63165946910083,9.29710969756502));
#23109=CARTESIAN_POINT('Origin',(48.2394105756736,-3.63165946910083,20.6896511931003));
#23110=CARTESIAN_POINT('Origin',(48.2394105756736,-3.63165946910083,20.6896511931003));
#23111=CARTESIAN_POINT('Origin',(48.2394105756736,-4.63165946910082,20.6896511931003));
#23112=CARTESIAN_POINT('Origin',(67.8495107361129,-3.63165946910083,7.38584475819711));
#23113=CARTESIAN_POINT('',(68.849510736113,-3.63165946910083,10.0458771867885));
#23114=CARTESIAN_POINT('',(68.8495107361129,-3.63165946910083,7.38584475819707));
#23115=CARTESIAN_POINT('Origin',(67.849510736113,-3.63165946910083,10.0458771867885));
#23116=CARTESIAN_POINT('',(67.8495107361129,-4.63165946910082,7.38584475819711));
#23117=CARTESIAN_POINT('Ctrl Pts',(68.849510736113,3.63165946910083,9.29710969756497));
#23118=CARTESIAN_POINT('Ctrl Pts',(68.849510736113,-5.08432325674117,9.29710969756497));
#23119=CARTESIAN_POINT('Ctrl Pts',(68.8495107361129,3.63165946910083,9.09090754844031));
#23120=CARTESIAN_POINT('Ctrl Pts',(68.8495107361129,-5.08432325674117,9.09090754844031));
#23121=CARTESIAN_POINT('Ctrl Pts',(68.7176416128359,3.63165946910083,8.67916780466697));
#23122=CARTESIAN_POINT('Ctrl Pts',(68.7176416128359,-5.08432325674117,8.67916780466697));
#23123=CARTESIAN_POINT('Ctrl Pts',(68.3717770285345,3.63165946910083,8.41975159159924));
#23124=CARTESIAN_POINT('Ctrl Pts',(68.3717770285345,-5.08432325674117,8.41975159159924));
#23125=CARTESIAN_POINT('Ctrl Pts',(68.1769417551904,3.63165946910083,8.3522346117754));
#23126=CARTESIAN_POINT('Ctrl Pts',(68.1769417551904,-5.08432325674117,8.3522346117754));
#23127=CARTESIAN_POINT('',(68.1769417551904,3.63165946910082,8.3522346117754));
#23128=CARTESIAN_POINT('',(68.1769417551904,-3.63165946910084,8.3522346117754));
#23129=CARTESIAN_POINT('',(68.849510736113,3.63165946910083,9.29710969756497));
#23130=CARTESIAN_POINT('Origin',(67.8495107361129,3.63165946910083,9.29710969756502));
#23131=CARTESIAN_POINT('',(68.849510736113,3.63165946910083,9.29710969756497));
#23132=CARTESIAN_POINT('Ctrl Pts',(60.3311054945567,4.63165946910082,5.02753578662844));
#23133=CARTESIAN_POINT('Ctrl Pts',(60.3311054945567,-6.48432325674116,5.02753578662844));
#23134=CARTESIAN_POINT('Ctrl Pts',(60.446720639058,4.63165946910082,5.10508973371974));
#23135=CARTESIAN_POINT('Ctrl Pts',(60.446720639058,-6.48432325674116,5.10508973371974));
#23136=CARTESIAN_POINT('Ctrl Pts',(60.6751612024229,4.63165946910082,5.256858542967));
#23137=CARTESIAN_POINT('Ctrl Pts',(60.6751612024229,-6.48432325674116,5.256858542967));
#23138=CARTESIAN_POINT('Ctrl Pts',(61.0094526814666,4.63165946910082,5.47449446266438));
#23139=CARTESIAN_POINT('Ctrl Pts',(61.0094526814666,-6.48432325674116,5.47449446266438));
#23140=CARTESIAN_POINT('Ctrl Pts',(61.4383158098093,4.63165946910082,5.74449578072259));
#23141=CARTESIAN_POINT('Ctrl Pts',(61.4383158098093,-6.48432325674116,5.74449578072259));
#23142=CARTESIAN_POINT('Ctrl Pts',(61.9466867115244,4.63165946910082,6.04793325275811));
#23143=CARTESIAN_POINT('Ctrl Pts',(61.9466867115244,-6.48432325674116,6.04793325275811));
#23144=CARTESIAN_POINT('Ctrl Pts',(62.4298628019368,4.63165946910082,6.31757162375642));
#23145=CARTESIAN_POINT('Ctrl Pts',(62.4298628019368,-6.48432325674116,6.31757162375642));
#23146=CARTESIAN_POINT('Ctrl Pts',(62.8939157006416,4.63165946910082,6.55518883032436));
#23147=CARTESIAN_POINT('Ctrl Pts',(62.8939157006416,-6.48432325674116,6.55518883032436));
#23148=CARTESIAN_POINT('Ctrl Pts',(63.3503010803271,4.63165946910082,6.76511373244055));
#23149=CARTESIAN_POINT('Ctrl Pts',(63.3503010803271,-6.48432325674116,6.76511373244055));
#23150=CARTESIAN_POINT('Ctrl Pts',(63.817162452721,4.63165946910082,6.95510921550471));
#23151=CARTESIAN_POINT('Ctrl Pts',(63.817162452721,-6.48432325674116,6.95510921550471));
#23152=CARTESIAN_POINT('Ctrl Pts',(64.3144171869106,4.63165946910082,7.13456216129536));
#23153=CARTESIAN_POINT('Ctrl Pts',(64.3144171869106,-6.48432325674116,7.13456216129536));
#23154=CARTESIAN_POINT('Ctrl Pts',(64.8590020041975,4.63165946910082,7.3128881543301));
#23155=CARTESIAN_POINT('Ctrl Pts',(64.8590020041975,-6.48432325674116,7.3128881543301));
#23156=CARTESIAN_POINT('Ctrl Pts',(65.4606023841754,4.63165946910082,7.4980830923353));
#23157=CARTESIAN_POINT('Ctrl Pts',(65.4606023841754,-6.48432325674116,7.4980830923353));
#23158=CARTESIAN_POINT('Ctrl Pts',(66.1152065663236,4.63165946910082,7.69478569974882));
#23159=CARTESIAN_POINT('Ctrl Pts',(66.1152065663236,-6.48432325674116,7.69478569974882));
#23160=CARTESIAN_POINT('Ctrl Pts',(66.8054984748247,4.63165946910082,7.90406632490002));
#23161=CARTESIAN_POINT('Ctrl Pts',(66.8054984748247,-6.48432325674116,7.90406632490002));
#23162=CARTESIAN_POINT('Ctrl Pts',(67.5081873326985,4.63165946910082,8.12495539290683));
#23163=CARTESIAN_POINT('Ctrl Pts',(67.5081873326985,-6.48432325674116,8.12495539290683));
#23164=CARTESIAN_POINT('Ctrl Pts',(68.060936927539,4.63165946910082,8.30930757589414));
#23165=CARTESIAN_POINT('Ctrl Pts',(68.060936927539,-6.48432325674116,8.30930757589414));
#23166=CARTESIAN_POINT('Ctrl Pts',(68.4616084894291,4.63165946910082,8.45095277650561));
#23167=CARTESIAN_POINT('Ctrl Pts',(68.4616084894291,-6.48432325674116,8.45095277650561));
#23168=CARTESIAN_POINT('Ctrl Pts',(68.7214260781516,4.63165946910082,8.54674866119352));
#23169=CARTESIAN_POINT('Ctrl Pts',(68.7214260781516,-6.48432325674116,8.54674866119352));
#23170=CARTESIAN_POINT('Ctrl Pts',(68.8495107361129,4.63165946910082,8.59498806995077));
#23171=CARTESIAN_POINT('Ctrl Pts',(68.8495107361129,-6.48432325674116,8.59498806995077));
#23172=CARTESIAN_POINT('',(60.3311081584417,3.63165946910082,5.02753777349255));
#23173=CARTESIAN_POINT('',(60.3311054945567,-3.63165946910082,5.02753578662843));
#23174=CARTESIAN_POINT('Ctrl Pts',(68.1769417551904,3.63165946910082,8.35223461177543));
#23175=CARTESIAN_POINT('Ctrl Pts',(68.0448580891249,3.63165946910082,8.30646317591714));
#23176=CARTESIAN_POINT('Ctrl Pts',(67.774992316996,3.63165946910082,8.21465783622081));
#23177=CARTESIAN_POINT('Ctrl Pts',(67.3615861901275,3.63165946910082,8.07887174821204));
#23178=CARTESIAN_POINT('Ctrl Pts',(66.8025201331148,3.63165946910082,7.90316336021611));
#23179=CARTESIAN_POINT('Ctrl Pts',(66.1152065663236,3.63165946910082,7.69478569974882));
#23180=CARTESIAN_POINT('Ctrl Pts',(65.4606023841754,3.63165946910082,7.4980830923353));
#23181=CARTESIAN_POINT('Ctrl Pts',(64.8590020041975,3.63165946910082,7.3128881543301));
#23182=CARTESIAN_POINT('Ctrl Pts',(64.3144171869106,3.63165946910082,7.13456216129536));
#23183=CARTESIAN_POINT('Ctrl Pts',(63.817162452721,3.63165946910082,6.95510921550471));
#23184=CARTESIAN_POINT('Ctrl Pts',(63.3503010803271,3.63165946910082,6.76511373244055));
#23185=CARTESIAN_POINT('Ctrl Pts',(62.8939157006416,3.63165946910082,6.55518883032436));
#23186=CARTESIAN_POINT('Ctrl Pts',(62.4298628019368,3.63165946910082,6.31757162375642));
#23187=CARTESIAN_POINT('Ctrl Pts',(61.9466867115244,3.63165946910082,6.04793325275811));
#23188=CARTESIAN_POINT('Ctrl Pts',(61.438316294613,3.63165946910082,5.74449607009322));
#23189=CARTESIAN_POINT('Ctrl Pts',(61.009453703921,3.63165946910082,5.47449510637563));
#23190=CARTESIAN_POINT('Ctrl Pts',(60.6751627963943,3.63165946910082,5.25685958070033));
#23191=CARTESIAN_POINT('Ctrl Pts',(60.4467228175623,3.63165946910082,5.10509118105016));
#23192=CARTESIAN_POINT('Ctrl Pts',(60.331108250942,3.63165946910082,5.02753763559501));
#23193=CARTESIAN_POINT('Origin',(67.849510736113,-3.63165946910083,10.0458771867885));
#23194=CARTESIAN_POINT('Origin',(67.849510736113,-3.63165946910083,10.0458771867885));
#23195=CARTESIAN_POINT('Origin',(57.5530637513316,-4.63165946910082,6.17670144644389));
#23196=CARTESIAN_POINT('Origin',(48.2394105756736,3.63165946910083,20.6896511931003));
#23197=CARTESIAN_POINT('Ctrl Pts',(59.7460107289856,4.63165946910082,5.83920248277122));
#23198=CARTESIAN_POINT('Ctrl Pts',(59.7484213663643,4.63165946910082,5.83791349517356));
#23199=CARTESIAN_POINT('Ctrl Pts',(59.7508238157325,4.63165013641957,5.83661272220212));
#23200=CARTESIAN_POINT('Ctrl Pts',(59.8344558547524,4.63099371608051,5.79074099515917));
#23201=CARTESIAN_POINT('Ctrl Pts',(59.8918098938637,4.61969837883588,5.74011401798109));
#23202=CARTESIAN_POINT('Ctrl Pts',(59.9847123908258,4.58714974455729,5.6393735456099));
#23203=CARTESIAN_POINT('Ctrl Pts',(60.023677918704,4.56201831623123,5.58129068542543));
#23204=CARTESIAN_POINT('Ctrl Pts',(60.1055318301292,4.47921911226623,5.4311154386434));
#23205=CARTESIAN_POINT('Ctrl Pts',(60.1366831105316,4.41377764901186,5.34222783627159));
#23206=CARTESIAN_POINT('Ctrl Pts',(60.2158981698528,4.22648244644917,5.16679346746808));
#23207=CARTESIAN_POINT('Ctrl Pts',(60.2573225934332,4.12722090972173,5.13360448598749));
#23208=CARTESIAN_POINT('Ctrl Pts',(60.2972984071676,4.0012706276777,5.08700751139042));
#23209=CARTESIAN_POINT('Ctrl Pts',(60.3125822841339,3.93012447294352,5.06701348081299));
#23210=CARTESIAN_POINT('Ctrl Pts',(60.3301404264941,3.77717862934284,5.0360516928879));
#23211=CARTESIAN_POINT('Ctrl Pts',(60.3311107648635,3.70172097050662,5.02753985548907));
#23212=CARTESIAN_POINT('Ctrl Pts',(60.3311107648635,3.63165946910082,5.02753985548906));
#23213=CARTESIAN_POINT('Origin',(48.2394105756736,3.63165946910083,20.6896511931003));
#23214=CARTESIAN_POINT('Ctrl Pts',(59.746010728986,4.63165946910082,5.83920248277193));
#23215=CARTESIAN_POINT('Ctrl Pts',(59.7553520150816,4.63165946910082,5.84546856158671));
#23216=CARTESIAN_POINT('Ctrl Pts',(59.7646938885029,4.63165946910082,5.85173542775135));
#23217=CARTESIAN_POINT('Ctrl Pts',(60.2628303227855,4.63165946910084,6.1858477117844));
#23218=CARTESIAN_POINT('Ctrl Pts',(61.2531647920567,4.63165946910082,6.82066652204582));
#23219=CARTESIAN_POINT('Ctrl Pts',(62.8100479900584,4.63165946910083,7.66426081171851));
#23220=CARTESIAN_POINT('Ctrl Pts',(64.4774359515706,4.63165946910083,8.25725916914412));
#23221=CARTESIAN_POINT('Ctrl Pts',(66.1709303349025,4.63165946910083,8.74915286435064));
#23222=CARTESIAN_POINT('Ctrl Pts',(67.2933262825326,4.63165946910082,9.10437306478713));
#23223=CARTESIAN_POINT('Ctrl Pts',(67.8495107361129,4.63165946910082,9.29710969756502));
#23224=CARTESIAN_POINT('Ctrl Pts',(59.9126859546861,4.63165946910083,5.59072795598318));
#23225=CARTESIAN_POINT('Ctrl Pts',(59.9218878363471,4.63165946910083,5.59691875304915));
#23226=CARTESIAN_POINT('Ctrl Pts',(59.9315252774069,4.63165946910082,5.60334758552559));
#23227=CARTESIAN_POINT('Ctrl Pts',(60.4247295228265,4.63165946910084,5.93438604629096));
#23228=CARTESIAN_POINT('Ctrl Pts',(61.4103568228254,4.63165946910082,6.56549663438234));
#23229=CARTESIAN_POINT('Ctrl Pts',(62.932177315481,4.63165946910083,7.38990007808402));
#23230=CARTESIAN_POINT('Ctrl Pts',(64.5615716916243,4.63165946910083,7.96968276822744));
#23231=CARTESIAN_POINT('Ctrl Pts',(66.2581057498348,4.63165946910083,8.46323709414939));
#23232=CARTESIAN_POINT('Ctrl Pts',(67.3846557023474,4.63165946910082,8.81926326169801));
#23233=CARTESIAN_POINT('Ctrl Pts',(67.9474778679311,4.63165946910082,9.01440373298629));
#23234=CARTESIAN_POINT('Ctrl Pts',(60.2011742942814,4.38041846956978,5.16065801989078));
#23235=CARTESIAN_POINT('Ctrl Pts',(60.2104574730015,4.38041846956978,5.16689271932467));
#23236=CARTESIAN_POINT('Ctrl Pts',(60.2200229569978,4.38041846956978,5.17329320559942));
#23237=CARTESIAN_POINT('Ctrl Pts',(60.7084670242163,4.3804184695698,5.50109683581841));
#23238=CARTESIAN_POINT('Ctrl Pts',(61.6806422694785,4.38041846956978,6.12294125446242));
#23239=CARTESIAN_POINT('Ctrl Pts',(63.1462916844765,4.38041846956979,6.91644720799102));
#23240=CARTESIAN_POINT('Ctrl Pts',(64.7063856583534,4.38041846956978,7.4716056430184));
#23241=CARTESIAN_POINT('Ctrl Pts',(66.4093830193833,4.38041846956978,7.9685837608805));
#23242=CARTESIAN_POINT('Ctrl Pts',(67.5450516434801,4.38041846956978,8.32682701341114));
#23243=CARTESIAN_POINT('Ctrl Pts',(68.1170434111871,4.38041846956978,8.52508461568826));
#23244=CARTESIAN_POINT('Ctrl Pts',(60.3030816362697,3.85605894435724,5.0087375501841));
#23245=CARTESIAN_POINT('Ctrl Pts',(60.3124229223653,3.85605894435724,5.01500362899888));
#23246=CARTESIAN_POINT('Ctrl Pts',(60.3219098237078,3.85605894435724,5.02136597894065));
#23247=CARTESIAN_POINT('Ctrl Pts',(60.8090164554297,3.85605894435727,5.34821691824898));
#23248=CARTESIAN_POINT('Ctrl Pts',(61.7759565243552,3.85605894435724,5.96652864430215));
#23249=CARTESIAN_POINT('Ctrl Pts',(63.2221752516257,3.85605894435725,6.74933144341603));
#23250=CARTESIAN_POINT('Ctrl Pts',(64.7574666625901,3.85605894435724,7.29563202006918));
#23251=CARTESIAN_POINT('Ctrl Pts',(66.462856679228,3.85605894435724,7.79386964203506));
#23252=CARTESIAN_POINT('Ctrl Pts',(67.6019221589542,3.85605894435724,8.15297096812908));
#23253=CARTESIAN_POINT('Ctrl Pts',(68.1769417551904,3.85605894435724,8.3522346117754));
#23254=CARTESIAN_POINT('Ctrl Pts',(60.3030816362697,3.63165946910083,5.0087375501841));
#23255=CARTESIAN_POINT('Ctrl Pts',(60.3124229223653,3.63165946910083,5.01500362899888));
#23256=CARTESIAN_POINT('Ctrl Pts',(60.3219098237078,3.63165946910082,5.02136597894065));
#23257=CARTESIAN_POINT('Ctrl Pts',(60.8090164554297,3.63165946910086,5.34821691824898));
#23258=CARTESIAN_POINT('Ctrl Pts',(61.7759565243552,3.63165946910082,5.96652864430215));
#23259=CARTESIAN_POINT('Ctrl Pts',(63.2221752516257,3.63165946910084,6.74933144341603));
#23260=CARTESIAN_POINT('Ctrl Pts',(64.7574666625901,3.63165946910083,7.29563202006918));
#23261=CARTESIAN_POINT('Ctrl Pts',(66.462856679228,3.63165946910083,7.79386964203506));
#23262=CARTESIAN_POINT('Ctrl Pts',(67.6019221589542,3.63165946910082,8.15297096812908));
#23263=CARTESIAN_POINT('Ctrl Pts',(68.1769417551904,3.63165946910082,8.3522346117754));
#23264=CARTESIAN_POINT('Origin',(67.8495107361129,3.63165946910082,9.29710969756502));
#23265=CARTESIAN_POINT('Origin',(67.8495107361129,3.63165946910083,9.29710969756502));
#23266=CARTESIAN_POINT('Origin',(67.8495107361129,3.63165946910083,9.29710969756502));
#23267=CARTESIAN_POINT('Origin',(67.8495107361129,3.63165946910083,7.38584475819711));
#23268=CARTESIAN_POINT('',(68.849510736113,3.63165946910083,10.0458771867885));
#23269=CARTESIAN_POINT('Origin',(67.849510736113,3.63165946910083,10.0458771867885));
#23270=CARTESIAN_POINT('',(68.8495107361129,3.63165946910083,7.38584475819707));
#23271=CARTESIAN_POINT('Origin',(67.849510736113,3.63165946910083,10.0458771867885));
#23272=CARTESIAN_POINT('Origin',(67.849510736113,3.63165946910083,10.0458771867885));
#23273=CARTESIAN_POINT('Origin',(67.849510736113,-3.63165946910082,10.0458771867885));
#23274=CARTESIAN_POINT('',(68.849510736113,-3.63165946910082,10.0458771867885));
#23275=CARTESIAN_POINT('Origin',(68.8495107361129,-3.63165946910082,8.59498806995077));
#23276=CARTESIAN_POINT('Origin',(57.5530637513316,3.63165946910082,6.17670144644389));
#23277=CARTESIAN_POINT('',(68.403087843053,3.63165946910082,8.90436665637973));
#23278=CARTESIAN_POINT('Ctrl Pts',(68.4030878430529,3.63165946910082,8.90436665637969));
#23279=CARTESIAN_POINT('Ctrl Pts',(68.1524251884716,3.63165946910082,8.81037448856025));
#23280=CARTESIAN_POINT('Ctrl Pts',(67.9114447001595,3.63165946910082,8.72240948548772));
#23281=CARTESIAN_POINT('Ctrl Pts',(67.6801396594394,3.63165946910082,8.64046105199615));
#23282=CARTESIAN_POINT('Ctrl Pts',(67.5033958661816,3.63165946910082,8.57784297440588));
#23283=CARTESIAN_POINT('Ctrl Pts',(67.3323019740517,3.63165946910082,8.5187384505674));
#23284=CARTESIAN_POINT('Ctrl Pts',(67.1668319793641,3.63165946910082,8.46311503412855));
#23285=CARTESIAN_POINT('Ctrl Pts',(67.0167717767144,3.63165946910082,8.41267168239798));
#23286=CARTESIAN_POINT('Ctrl Pts',(66.8713371061142,3.63165946910082,8.36509159944541));
#23287=CARTESIAN_POINT('Ctrl Pts',(66.7304811603576,3.63165946910082,8.32031886206648));
#23288=CARTESIAN_POINT('Ctrl Pts',(66.5991138318065,3.63165946910082,8.27856219450235));
#23289=CARTESIAN_POINT('Ctrl Pts',(66.471729349538,3.63165946910082,8.23924762412635));
#23290=CARTESIAN_POINT('Ctrl Pts',(66.3482609420148,3.63165946910082,8.2022969215945));
#23291=CARTESIAN_POINT('Ctrl Pts',(66.2311942728027,3.63165946910082,8.16726208347499));
#23292=CARTESIAN_POINT('Ctrl Pts',(66.1176483084088,3.63165946910082,8.13435255477346));
#23293=CARTESIAN_POINT('Ctrl Pts',(66.0075362307229,3.63165946910082,8.10346765416841));
#23294=CARTESIAN_POINT('Ctrl Pts',(65.9012263499085,3.63165946910082,8.07364921670638));
#23295=CARTESIAN_POINT('Ctrl Pts',(65.7981174703656,3.63165946910082,8.04571817981046));
#23296=CARTESIAN_POINT('Ctrl Pts',(65.6981000899904,3.63165946910082,8.01954833389659));
#23297=CARTESIAN_POINT('Ctrl Pts',(65.6006424733329,3.63165946910082,7.99404825779491));
#23298=CARTESIAN_POINT('Ctrl Pts',(65.5061202399805,3.63165946910082,7.97022047197159));
#23299=CARTESIAN_POINT('Ctrl Pts',(65.4143999331461,3.63165946910082,7.94791197409409));
#23300=CARTESIAN_POINT('Ctrl Pts',(65.3255799119656,3.63165946910082,7.92630889270057));
#23301=CARTESIAN_POINT('Ctrl Pts',(65.2393874705361,3.63165946910082,7.90613058034837));
#23302=CARTESIAN_POINT('Ctrl Pts',(65.1556698865984,3.63165946910082,7.88720280343498));
#23303=CARTESIAN_POINT('Ctrl Pts',(65.07506789503,3.63165946910082,7.86897943334443));
#23304=CARTESIAN_POINT('Ctrl Pts',(64.9967601069725,3.63165946910082,7.85191541352309));
#23305=CARTESIAN_POINT('Ctrl Pts',(64.9205792020063,3.63165946910082,7.83582042303275));
#23306=CARTESIAN_POINT('Ctrl Pts',(64.846118138096,3.63165946910082,7.820088789022));
#23307=CARTESIAN_POINT('Ctrl Pts',(64.7736891723661,3.63165946910082,7.80528312708477));
#23308=CARTESIAN_POINT('Ctrl Pts',(64.7031036424093,3.63165946910082,7.79118902409658));
#23309=CARTESIAN_POINT('Ctrl Pts',(64.6312305851568,3.63165946910082,7.77683783523942));
#23310=CARTESIAN_POINT('Ctrl Pts',(64.5612688955538,3.63165946910082,7.76322441576092));
#23311=CARTESIAN_POINT('Ctrl Pts',(64.492982491524,3.63165946910082,7.7500807655258));
#23312=CARTESIAN_POINT('Ctrl Pts',(64.4224488831997,3.63165946910082,7.73650457725223));
#23313=CARTESIAN_POINT('Ctrl Pts',(64.3537025897904,3.63165946910082,7.72342940546561));
#23314=CARTESIAN_POINT('Ctrl Pts',(64.2864447162966,3.63165946910082,7.71051780525175));
#23315=CARTESIAN_POINT('Ctrl Pts',(64.2131307134005,3.63165946910082,7.69644360031038));
#23316=CARTESIAN_POINT('Ctrl Pts',(64.1415853319417,3.63165946910082,7.68256356416357));
#23317=CARTESIAN_POINT('Ctrl Pts',(64.071374458361,3.63165946910082,7.66839258437265));
#23318=CARTESIAN_POINT('Ctrl Pts',(63.9812801976944,3.63165946910082,7.65020845017701));
#23319=CARTESIAN_POINT('Ctrl Pts',(63.8933827141527,3.63165946910082,7.63154252215813));
#23320=CARTESIAN_POINT('Ctrl Pts',(63.8066895419125,3.63165946910082,7.61131155332181));
#23321=CARTESIAN_POINT('Ctrl Pts',(63.728322356967,3.63165946910082,7.5930235609061));
#23322=CARTESIAN_POINT('Ctrl Pts',(63.6509358784921,3.63165946910082,7.57345251495131));
#23323=CARTESIAN_POINT('Ctrl Pts',(63.57378242349,3.63165946910082,7.55181695935026));
#23324=CARTESIAN_POINT('Ctrl Pts',(63.5094090616368,3.63165946910082,7.53376522790721));
#23325=CARTESIAN_POINT('Ctrl Pts',(63.4451971003337,3.63165946910082,7.51427577290783));
#23326=CARTESIAN_POINT('Ctrl Pts',(63.3807236660863,3.63165946910082,7.49293131763497));
#23327=CARTESIAN_POINT('Ctrl Pts',(63.3224846953064,3.63165946910082,7.47365083224652));
#23328=CARTESIAN_POINT('Ctrl Pts',(63.2640320091646,3.63165946910082,7.45285644728535));
#23329=CARTESIAN_POINT('Ctrl Pts',(63.2050711081345,3.63165946910082,7.43027832497762));
#23330=CARTESIAN_POINT('Ctrl Pts',(63.1502701886774,3.63165946910082,7.40929320025156));
#23331=CARTESIAN_POINT('Ctrl Pts',(63.0950299666058,3.63165946910082,7.38676687657799));
#23332=CARTESIAN_POINT('Ctrl Pts',(63.0391341137597,3.63165946910082,7.36252141714122));
#23333=CARTESIAN_POINT('Ctrl Pts',(62.9856894260991,3.63165946910082,7.33933917837381));
#23334=CARTESIAN_POINT('Ctrl Pts',(62.9316451194371,3.63165946910082,7.31458499408552));
#23335=CARTESIAN_POINT('Ctrl Pts',(62.8768347758996,3.63165946910082,7.28814419321545));
#23336=CARTESIAN_POINT('Ctrl Pts',(62.821749297725,3.63165946910082,7.26157066593498));
#23337=CARTESIAN_POINT('Ctrl Pts',(62.7658899881053,3.63165946910082,7.23329348079273));
#23338=CARTESIAN_POINT('Ctrl Pts',(62.7091146273812,3.63165946910082,7.20324266246051));
#23339=CARTESIAN_POINT('Ctrl Pts',(62.6513638361753,3.63165946910082,7.17267555530464));
#23340=CARTESIAN_POINT('Ctrl Pts',(62.5926652593515,3.63165946910082,7.14027344884607));
#23341=CARTESIAN_POINT('Ctrl Pts',(62.5328969217323,3.63165946910082,7.10600964833574));
#23342=CARTESIAN_POINT('Ctrl Pts',(62.4718828857829,3.63165946910082,7.07103171789008));
#23343=CARTESIAN_POINT('Ctrl Pts',(62.4097540366417,3.63165946910082,7.03411378207533));
#23344=CARTESIAN_POINT('Ctrl Pts',(62.3464091406167,3.63165946910082,6.99527446217524));
#23345=CARTESIAN_POINT('Ctrl Pts',(62.2811210251423,3.63165946910082,6.95524367577082));
#23346=CARTESIAN_POINT('Ctrl Pts',(62.2145411445452,3.63165946910082,6.91317198799666));
#23347=CARTESIAN_POINT('Ctrl Pts',(62.1465884817725,3.63165946910082,6.86912731598505));
#23348=CARTESIAN_POINT('Ctrl Pts',(62.0761205275452,3.63165946910082,6.82345231511491));
#23349=CARTESIAN_POINT('Ctrl Pts',(62.0041763233329,3.63165946910082,6.7756557855778));
#23350=CARTESIAN_POINT('Ctrl Pts',(61.9306965406046,3.63165946910082,6.72586077918759));
#23351=CARTESIAN_POINT('Ctrl Pts',(61.8540789578711,3.63165946910082,6.67393938148928));
#23352=CARTESIAN_POINT('Ctrl Pts',(61.7757918913736,3.63165946910082,6.61984545880833));
#23353=CARTESIAN_POINT('Ctrl Pts',(61.6958005596679,3.63165946910082,6.56376514048228));
#23354=CARTESIAN_POINT('Ctrl Pts',(61.6117739636066,3.63165946910082,6.50485577924902));
#23355=CARTESIAN_POINT('Ctrl Pts',(61.5258668448555,3.63165946910082,6.44375490099631));
#23356=CARTESIAN_POINT('Ctrl Pts',(61.4380735612011,3.63165946910082,6.38072390991561));
#23357=CARTESIAN_POINT('Ctrl Pts',(61.3405968077594,3.63165946910082,6.31074069342094));
#23358=CARTESIAN_POINT('Ctrl Pts',(61.2407946053347,3.63165946910082,6.23837837095361));
#23359=CARTESIAN_POINT('Ctrl Pts',(61.1387033051201,3.63165946910082,6.16404542577452));
#23360=CARTESIAN_POINT('Ctrl Pts',(61.0257726543044,3.63165946910082,6.08182032080983));
#23361=CARTESIAN_POINT('Ctrl Pts',(60.9100409429449,3.63165946910082,5.99718492622526));
#23362=CARTESIAN_POINT('Ctrl Pts',(60.7916116265055,3.63165946910082,5.910741059164));
#23363=CARTESIAN_POINT('Ctrl Pts',(60.6580479108045,3.63165946910082,5.81325029900941));
#23364=CARTESIAN_POINT('Ctrl Pts',(60.5210532648285,3.63165946910082,5.71346202414252));
#23365=CARTESIAN_POINT('Ctrl Pts',(60.3808417449914,3.63165946910082,5.61226971445713));
#23366=CARTESIAN_POINT('Ctrl Pts',(60.2543711859363,3.63165946910082,5.52099441844102));
#23367=CARTESIAN_POINT('Ctrl Pts',(60.1252852457356,3.63165946910082,5.42857957892073));
#23368=CARTESIAN_POINT('Ctrl Pts',(59.9937718372108,3.63165946910082,5.33566159665948));
#23369=CARTESIAN_POINT('Ctrl Pts',(59.8714966547022,3.63165946910082,5.24927068514123));
#23370=CARTESIAN_POINT('Ctrl Pts',(59.7471238625868,3.63165946910082,5.16244575286178));
#23371=CARTESIAN_POINT('Ctrl Pts',(59.6208147984602,3.63165946910082,5.07565516314998));
#23372=CARTESIAN_POINT('Ctrl Pts',(59.4982169131285,3.63165946910082,4.99141463109531));
#23373=CARTESIAN_POINT('Ctrl Pts',(59.3737951905991,3.63165946910082,4.90720667908688));
#23374=CARTESIAN_POINT('Ctrl Pts',(59.247700268628,3.63165946910082,4.82341149904876));
#23375=CARTESIAN_POINT('Ctrl Pts',(59.1205071392074,3.63165946910082,4.73888651570445));
#23376=CARTESIAN_POINT('Ctrl Pts',(58.9916117176436,3.63165946910082,4.65478168438331));
#23377=CARTESIAN_POINT('Ctrl Pts',(58.8611677026219,3.63165946910082,4.57143304088211));
#23378=CARTESIAN_POINT('Ctrl Pts',(58.7268954605109,3.63165946910082,4.48563830941861));
#23379=CARTESIAN_POINT('Ctrl Pts',(58.5909824288711,3.63165946910082,4.4006446245073));
#23380=CARTESIAN_POINT('Ctrl Pts',(58.4535940638078,3.63165946910082,4.31676247264537));
#23381=CARTESIAN_POINT('Ctrl Pts',(58.3135767950974,3.63165946910082,4.23127524967813));
#23382=CARTESIAN_POINT('Ctrl Pts',(58.172027277087,3.63165946910082,4.14694233221852));
#23383=CARTESIAN_POINT('Ctrl Pts',(58.0291176860168,3.63165946910082,4.06403836576243));
#23384=CARTESIAN_POINT('Ctrl Pts',(57.8844984402709,3.63165946910082,3.9801426033546));
#23385=CARTESIAN_POINT('Ctrl Pts',(57.7384865353406,3.63165946910083,3.8977101052527));
#23386=CARTESIAN_POINT('Ctrl Pts',(57.5912554524475,3.63165946910083,3.81697225280899));
#23387=CARTESIAN_POINT('Ctrl Pts',(57.4411855775284,3.63165946910083,3.73467767764605));
#23388=CARTESIAN_POINT('Ctrl Pts',(57.2898492019476,3.63165946910083,3.65414360653815));
#23389=CARTESIAN_POINT('Ctrl Pts',(57.1374225697492,3.63165946910083,3.575561274548));
#23390=CARTESIAN_POINT('Ctrl Pts',(56.9812329132406,3.63165946910083,3.49503894544995));
#23391=CARTESIAN_POINT('Ctrl Pts',(56.82389865689,3.63165946910083,3.41656573389789));
#23392=CARTESIAN_POINT('Ctrl Pts',(56.6655994249122,3.63165946910083,3.340293868234));
#23393=CARTESIAN_POINT('Ctrl Pts',(56.501946506452,3.63165946910083,3.2614424849623));
#23394=CARTESIAN_POINT('Ctrl Pts',(56.3372624700534,3.63165946910083,3.18494377213621));
#23395=CARTESIAN_POINT('Ctrl Pts',(56.1717322849393,3.63165946910083,3.11091154608564));
#23396=CARTESIAN_POINT('Ctrl Pts',(56.0024276869476,3.63165946910083,3.03519124008049));
#23397=CARTESIAN_POINT('Ctrl Pts',(55.8322381664413,3.63165946910083,2.96205096200203));
#23398=CARTESIAN_POINT('Ctrl Pts',(55.6613439821123,3.63165946910083,2.89155902627219));
#23399=CARTESIAN_POINT('Ctrl Pts',(55.4861649710066,3.63165946910083,2.81929964751945));
#23400=CARTESIAN_POINT('Ctrl Pts',(55.3102457891247,3.63165946910083,2.74982277944709));
#23401=CARTESIAN_POINT('Ctrl Pts',(55.1337581760356,3.63165946910083,2.68315043469479));
#23402=CARTESIAN_POINT('Ctrl Pts',(54.9532225222413,3.63165946910083,2.61494884740395));
#23403=CARTESIAN_POINT('Ctrl Pts',(54.7720923867629,3.63165946910083,2.54968152006114));
#23404=CARTESIAN_POINT('Ctrl Pts',(54.5905239270766,3.63165946910083,2.48732409656624));
#23405=CARTESIAN_POINT('Ctrl Pts',(54.4052967110213,3.63165946910083,2.42371011881756));
#23406=CARTESIAN_POINT('Ctrl Pts',(54.2196137418316,3.63165946910082,2.36312402272515));
#23407=CARTESIAN_POINT('Ctrl Pts',(54.0336065701925,3.63165946910082,2.30549732676221));
#23408=CARTESIAN_POINT('Ctrl Pts',(53.8387224059876,3.63165946910082,2.24512045860351));
#23409=CARTESIAN_POINT('Ctrl Pts',(53.6434823245496,3.63165946910083,2.18799183172259));
#23410=CARTESIAN_POINT('Ctrl Pts',(53.4479954020231,3.63165946910083,2.13399288221745));
#23411=CARTESIAN_POINT('Ctrl Pts',(53.2249151702052,3.63165946910083,2.07237188978564));
#23412=CARTESIAN_POINT('Ctrl Pts',(53.0015135292926,3.63165946910083,2.01482634101555));
#23413=CARTESIAN_POINT('Ctrl Pts',(52.7778983586911,3.63165946910083,1.96113227115105));
#23414=CARTESIAN_POINT('Ctrl Pts',(52.5225551474507,3.63165946910083,1.89981972161835));
#23415=CARTESIAN_POINT('Ctrl Pts',(52.2669323001051,3.63165946910083,1.84352809056697));
#23416=CARTESIAN_POINT('Ctrl Pts',(52.0111327763155,3.63165946910083,1.79187414000036));
#23417=CARTESIAN_POINT('Ctrl Pts',(51.7291129942993,3.63165946910083,1.73492549653435));
#23418=CARTESIAN_POINT('Ctrl Pts',(51.4468750698643,3.63165946910083,1.68361086005454));
#23419=CARTESIAN_POINT('Ctrl Pts',(51.1645293729854,3.63165946910083,1.63739431772361));
#23420=CARTESIAN_POINT('Ctrl Pts',(50.9361416709355,3.63165946910083,1.60001004016484));
#23421=CARTESIAN_POINT('Ctrl Pts',(50.7076817864648,3.63165946910083,1.5659600732803));
#23422=CARTESIAN_POINT('Ctrl Pts',(50.4792240082351,3.63165946910083,1.53497655175055));
#23423=CARTESIAN_POINT('Ctrl Pts',(50.2700379291693,3.63165946910083,1.50660666461129));
#23424=CARTESIAN_POINT('Ctrl Pts',(50.0608529569732,3.63165946910083,1.48080711340197));
#23425=CARTESIAN_POINT('Ctrl Pts',(49.8517551192908,3.63165946910083,1.45739919122166));
#23426=CARTESIAN_POINT('Ctrl Pts',(49.648357764131,3.63165946910083,1.43462942222725));
#23427=CARTESIAN_POINT('Ctrl Pts',(49.4450421707224,3.63165946910083,1.41412203464256));
#23428=CARTESIAN_POINT('Ctrl Pts',(49.2419255557958,3.63165946910083,1.39574767539995));
#23429=CARTESIAN_POINT('Ctrl Pts',(49.0608871158299,3.63165946910083,1.37937055463186));
#23430=CARTESIAN_POINT('Ctrl Pts',(48.8800066915195,3.63165946910083,1.36468794115039));
#23431=CARTESIAN_POINT('Ctrl Pts',(48.6994022361495,3.63165946910082,1.35164010884257));
#23432=CARTESIAN_POINT('Ctrl Pts',(48.6773769868982,3.63165946910082,1.35004888697497));
#23433=CARTESIAN_POINT('Ctrl Pts',(48.6553558896734,3.63165946910082,1.34848202152824));
#23434=CARTESIAN_POINT('Ctrl Pts',(48.6333391993365,3.63165946910082,1.3469394411452));
#23435=CARTESIAN_POINT('',(68.4030878430531,3.63165946910082,10.8150451223525));
#23436=CARTESIAN_POINT('',(68.4030878430529,3.63165946910082,7.54053405141158));
#23437=CARTESIAN_POINT('Origin',(48.2463073637984,3.63165946910082,69.7993133400951));
#23438=CARTESIAN_POINT('Origin',(48.2463073637984,-3.63165946910082,69.7993133400951));
#23439=CARTESIAN_POINT('',(68.4030878430531,-3.63165946910082,10.8150451223525));
#23440=CARTESIAN_POINT('',(68.4030878430531,-3.63165946910082,10.8150451223525));
#23441=CARTESIAN_POINT('Origin',(48.2463073637984,-3.63165946910082,69.7993133400951));
#23442=CARTESIAN_POINT('Origin',(68.403087843053,-3.63165946910082,8.90436665637973));
#23443=CARTESIAN_POINT('',(68.403087843053,-3.63165946910082,8.90436665637973));
#23444=CARTESIAN_POINT('',(68.403087843053,-3.63165946910082,8.90436665637973));
#23445=CARTESIAN_POINT('',(68.4030878430529,-3.63165946910082,7.54053405141158));
#23446=CARTESIAN_POINT('Ctrl Pts',(48.6333391993365,-3.63165946910083,1.3469394411452));
#23447=CARTESIAN_POINT('Ctrl Pts',(48.6333391993365,5.68394053089918,1.3469394411452));
#23448=CARTESIAN_POINT('Ctrl Pts',(48.6559901910909,-3.63165946910083,1.34852646330893));
#23449=CARTESIAN_POINT('Ctrl Pts',(48.6559901910909,5.68394053089918,1.34852646330893));
#23450=CARTESIAN_POINT('Ctrl Pts',(48.8580826500258,-3.63165946910082,1.3628745531293));
#23451=CARTESIAN_POINT('Ctrl Pts',(48.8580826500258,5.68394053089919,1.3628745531293));
#23452=CARTESIAN_POINT('Ctrl Pts',(49.2401770875181,-3.63165946910082,1.3931854505195));
#23453=CARTESIAN_POINT('Ctrl Pts',(49.2401770875181,5.68394053089919,1.3931854505195));
#23454=CARTESIAN_POINT('Ctrl Pts',(49.8030694790913,-3.63165946910082,1.44683819965743));
#23455=CARTESIAN_POINT('Ctrl Pts',(49.8030694790913,5.68394053089919,1.44683819965743));
#23456=CARTESIAN_POINT('Ctrl Pts',(50.5469014142808,-3.63165946910082,1.53623826938649));
#23457=CARTESIAN_POINT('Ctrl Pts',(50.5469014142808,5.68394053089919,1.53623826938649));
#23458=CARTESIAN_POINT('Ctrl Pts',(51.4480843800216,-3.63165946910082,1.67655609650635));
#23459=CARTESIAN_POINT('Ctrl Pts',(51.4480843800216,5.68394053089919,1.67655609650635));
#23460=CARTESIAN_POINT('Ctrl Pts',(52.348266859532,-3.63165946910082,1.85267033982542));
#23461=CARTESIAN_POINT('Ctrl Pts',(52.348266859532,5.68394053089919,1.85267033982542));
#23462=CARTESIAN_POINT('Ctrl Pts',(53.2467046577141,-3.63165946910082,2.06850649471347));
#23463=CARTESIAN_POINT('Ctrl Pts',(53.2467046577141,5.68394053089919,2.06850649471347));
#23464=CARTESIAN_POINT('Ctrl Pts',(54.1422176988182,-3.63165946910082,2.32761261079463));
#23465=CARTESIAN_POINT('Ctrl Pts',(54.1422176988182,5.68394053089919,2.32761261079463));
#23466=CARTESIAN_POINT('Ctrl Pts',(55.0326050724517,-3.63165946910082,2.63265678969324));
#23467=CARTESIAN_POINT('Ctrl Pts',(55.0326050724517,5.68394053089919,2.63265678969324));
#23468=CARTESIAN_POINT('Ctrl Pts',(55.9141550877392,-3.63165946910082,2.98491249335729));
#23469=CARTESIAN_POINT('Ctrl Pts',(55.9141550877392,5.68394053089919,2.98491249335729));
#23470=CARTESIAN_POINT('Ctrl Pts',(56.7819405807955,-3.63165946910082,3.3836558364077));
#23471=CARTESIAN_POINT('Ctrl Pts',(56.7819405807955,5.68394053089919,3.3836558364077));
#23472=CARTESIAN_POINT('Ctrl Pts',(57.6300359536437,-3.63165946910082,3.82554246975634));
#23473=CARTESIAN_POINT('Ctrl Pts',(57.6300359536437,5.68394053089919,3.82554246975634));
#23474=CARTESIAN_POINT('Ctrl Pts',(58.4517774296143,-3.63165946910082,4.30403237376386));
#23475=CARTESIAN_POINT('Ctrl Pts',(58.4517774296143,5.68394053089919,4.30403237376386));
#23476=CARTESIAN_POINT('Ctrl Pts',(59.2399671195477,-3.63165946910082,4.80867544303911));
#23477=CARTESIAN_POINT('Ctrl Pts',(59.2399671195477,5.68394053089919,4.80867544303911));
#23478=CARTESIAN_POINT('Ctrl Pts',(59.9871842641414,-3.63165946910082,5.32469977859742));
#23479=CARTESIAN_POINT('Ctrl Pts',(59.9871842641414,5.68394053089919,5.32469977859742));
#23480=CARTESIAN_POINT('Ctrl Pts',(60.6858451039897,-3.63165946910082,5.83183545124052));
#23481=CARTESIAN_POINT('Ctrl Pts',(60.6858451039897,5.68394053089919,5.83183545124052));
#23482=CARTESIAN_POINT('Ctrl Pts',(61.3291075829706,-3.63165946910082,6.30568784052758));
#23483=CARTESIAN_POINT('Ctrl Pts',(61.3291075829706,5.68394053089919,6.30568784052758));
#23484=CARTESIAN_POINT('Ctrl Pts',(61.9129286688635,-3.63165946910082,6.72264590044013));
#23485=CARTESIAN_POINT('Ctrl Pts',(61.9129286688635,5.68394053089919,6.72264590044013));
#23486=CARTESIAN_POINT('Ctrl Pts',(62.4378966914009,-3.63165946910082,7.06401270956655));
#23487=CARTESIAN_POINT('Ctrl Pts',(62.4378966914009,5.68394053089919,7.06401270956655));
#23488=CARTESIAN_POINT('Ctrl Pts',(62.9110626727188,-3.63165946910082,7.32028203996567));
#23489=CARTESIAN_POINT('Ctrl Pts',(62.9110626727188,5.68394053089919,7.32028203996567));
#23490=CARTESIAN_POINT('Ctrl Pts',(63.3480382061253,-3.63165946910082,7.49580221124892));
#23491=CARTESIAN_POINT('Ctrl Pts',(63.3480382061253,5.68394053089919,7.49580221124892));
#23492=CARTESIAN_POINT('Ctrl Pts',(63.7742575841079,-3.63165946910082,7.61203807956635));
#23493=CARTESIAN_POINT('Ctrl Pts',(63.7742575841079,5.68394053089919,7.61203807956635));
#23494=CARTESIAN_POINT('Ctrl Pts',(64.2192519841205,-3.63165946910082,7.69914552267219));
#23495=CARTESIAN_POINT('Ctrl Pts',(64.2192519841205,5.68394053089919,7.69914552267219));
#23496=CARTESIAN_POINT('Ctrl Pts',(64.712086468945,-3.63165946910082,7.78936630198725));
#23497=CARTESIAN_POINT('Ctrl Pts',(64.712086468945,5.68394053089919,7.78936630198725));
#23498=CARTESIAN_POINT('Ctrl Pts',(65.2754113430736,-3.63165946910082,7.90844857460236));
#23499=CARTESIAN_POINT('Ctrl Pts',(65.2754113430736,5.68394053089919,7.90844857460236));
#23500=CARTESIAN_POINT('Ctrl Pts',(65.9237039528771,-3.63165946910082,8.07283920347654));
#23501=CARTESIAN_POINT('Ctrl Pts',(65.9237039528771,5.68394053089919,8.07283920347654));
#23502=CARTESIAN_POINT('Ctrl Pts',(66.6557369297143,-3.63165946910082,8.28958012503505));
#23503=CARTESIAN_POINT('Ctrl Pts',(66.6557369297143,5.68394053089919,8.28958012503505));
#23504=CARTESIAN_POINT('Ctrl Pts',(67.3150092482541,-3.63165946910082,8.50886642156034));
#23505=CARTESIAN_POINT('Ctrl Pts',(67.3150092482541,5.68394053089919,8.50886642156034));
#23506=CARTESIAN_POINT('Ctrl Pts',(67.8492602326033,-3.63165946910082,8.69890399191604));
#23507=CARTESIAN_POINT('Ctrl Pts',(67.8492602326033,5.68394053089919,8.69890399191604));
#23508=CARTESIAN_POINT('Ctrl Pts',(68.2198703338295,-3.63165946910082,8.8356647155056));
#23509=CARTESIAN_POINT('Ctrl Pts',(68.2198703338295,5.68394053089919,8.8356647155056));
#23510=CARTESIAN_POINT('Ctrl Pts',(68.4030878430529,-3.63165946910082,8.90436665637969));
#23511=CARTESIAN_POINT('Ctrl Pts',(68.4030878430529,5.68394053089919,8.90436665637969));
#23512=CARTESIAN_POINT('Ctrl Pts',(68.4030878430529,-3.63165946910082,8.90436665637969));
#23513=CARTESIAN_POINT('Ctrl Pts',(68.2198703338295,-3.63165946910082,8.8356647155056));
#23514=CARTESIAN_POINT('Ctrl Pts',(67.8492602326033,-3.63165946910082,8.69890399191604));
#23515=CARTESIAN_POINT('Ctrl Pts',(67.3150092482541,-3.63165946910082,8.50886642156034));
#23516=CARTESIAN_POINT('Ctrl Pts',(66.6557369297143,-3.63165946910082,8.28958012503505));
#23517=CARTESIAN_POINT('Ctrl Pts',(65.9237039528771,-3.63165946910082,8.07283920347654));
#23518=CARTESIAN_POINT('Ctrl Pts',(65.2754113430736,-3.63165946910082,7.90844857460236));
#23519=CARTESIAN_POINT('Ctrl Pts',(64.712086468945,-3.63165946910082,7.78936630198725));
#23520=CARTESIAN_POINT('Ctrl Pts',(64.2192519841205,-3.63165946910082,7.69914552267219));
#23521=CARTESIAN_POINT('Ctrl Pts',(63.7742575841079,-3.63165946910082,7.61203807956635));
#23522=CARTESIAN_POINT('Ctrl Pts',(63.3480382061253,-3.63165946910082,7.49580221124892));
#23523=CARTESIAN_POINT('Ctrl Pts',(62.9110626727188,-3.63165946910082,7.32028203996567));
#23524=CARTESIAN_POINT('Ctrl Pts',(62.4378966914009,-3.63165946910082,7.06401270956655));
#23525=CARTESIAN_POINT('Ctrl Pts',(61.9129286688635,-3.63165946910082,6.72264590044013));
#23526=CARTESIAN_POINT('Ctrl Pts',(61.3291075829706,-3.63165946910082,6.30568784052758));
#23527=CARTESIAN_POINT('Ctrl Pts',(60.6858451039897,-3.63165946910082,5.83183545124052));
#23528=CARTESIAN_POINT('Ctrl Pts',(59.9871842641414,-3.63165946910082,5.32469977859742));
#23529=CARTESIAN_POINT('Ctrl Pts',(59.2399671195477,-3.63165946910082,4.80867544303911));
#23530=CARTESIAN_POINT('Ctrl Pts',(58.4517774296143,-3.63165946910082,4.30403237376386));
#23531=CARTESIAN_POINT('Ctrl Pts',(57.6300359536437,-3.63165946910082,3.82554246975634));
#23532=CARTESIAN_POINT('Ctrl Pts',(56.7819405807955,-3.63165946910082,3.3836558364077));
#23533=CARTESIAN_POINT('Ctrl Pts',(55.9141550877392,-3.63165946910082,2.98491249335729));
#23534=CARTESIAN_POINT('Ctrl Pts',(55.0326050724517,-3.63165946910082,2.63265678969324));
#23535=CARTESIAN_POINT('Ctrl Pts',(54.1422176988182,-3.63165946910082,2.32761261079463));
#23536=CARTESIAN_POINT('Ctrl Pts',(53.2467046577141,-3.63165946910082,2.06850649471347));
#23537=CARTESIAN_POINT('Ctrl Pts',(52.348266859532,-3.63165946910082,1.85267033982542));
#23538=CARTESIAN_POINT('Ctrl Pts',(51.4480843800216,-3.63165946910082,1.67655609650635));
#23539=CARTESIAN_POINT('Ctrl Pts',(50.5469014142808,-3.63165946910082,1.53623826938649));
#23540=CARTESIAN_POINT('Ctrl Pts',(49.8030694790913,-3.63165946910082,1.44683819965743));
#23541=CARTESIAN_POINT('Ctrl Pts',(49.2401770875181,-3.63165946910082,1.3931854505195));
#23542=CARTESIAN_POINT('Ctrl Pts',(48.8580826500258,-3.63165946910082,1.3628745531293));
#23543=CARTESIAN_POINT('Ctrl Pts',(48.6559901910909,-3.63165946910083,1.34852646330893));
#23544=CARTESIAN_POINT('Ctrl Pts',(48.6333391993365,-3.63165946910083,1.3469394411452));
#23545=CARTESIAN_POINT('Origin',(57.5530637513316,-3.63165946910082,6.17670144644389));
#23546=CARTESIAN_POINT('Origin',(48.2394105756736,-3.63165946910082,20.6896511931003));
#23547=CARTESIAN_POINT('',(0.,0.,0.));
#23548=CARTESIAN_POINT('',(0.,0.,0.));
#23549=CARTESIAN_POINT('',(0.,0.,0.));
#23550=CARTESIAN_POINT('',(0.,0.,0.));
#23551=CARTESIAN_POINT('',(0.,0.,0.));
#23552=CARTESIAN_POINT('',(0.,0.,0.));
#23553=CARTESIAN_POINT('',(0.,0.,0.));
#23554=CARTESIAN_POINT('',(0.,0.,0.));
#23555=CARTESIAN_POINT('',(0.,0.,0.));
#23556=UNCERTAINTY_MEASURE_WITH_UNIT(LENGTH_MEASURE(0.01),#23578,
'DISTANCE_ACCURACY_VALUE',
'Maximum model space distance between geometric entities at asserted c
onnectivities');
#23557=UNCERTAINTY_MEASURE_WITH_UNIT(LENGTH_MEASURE(0.01),#23578,
'DISTANCE_ACCURACY_VALUE',
'Maximum model space distance between geometric entities at asserted c
onnectivities');
#23558=UNCERTAINTY_MEASURE_WITH_UNIT(LENGTH_MEASURE(0.01),#23578,
'DISTANCE_ACCURACY_VALUE',
'Maximum model space distance between geometric entities at asserted c
onnectivities');
#23559=UNCERTAINTY_MEASURE_WITH_UNIT(LENGTH_MEASURE(0.01),#23578,
'DISTANCE_ACCURACY_VALUE',
'Maximum model space distance between geometric entities at asserted c
onnectivities');
#23560=UNCERTAINTY_MEASURE_WITH_UNIT(LENGTH_MEASURE(0.01),#23578,
'DISTANCE_ACCURACY_VALUE',
'Maximum model space distance between geometric entities at asserted c
onnectivities');
#23561=UNCERTAINTY_MEASURE_WITH_UNIT(LENGTH_MEASURE(0.01),#23578,
'DISTANCE_ACCURACY_VALUE',
'Maximum model space distance between geometric entities at asserted c
onnectivities');
#23562=UNCERTAINTY_MEASURE_WITH_UNIT(LENGTH_MEASURE(0.01),#23578,
'DISTANCE_ACCURACY_VALUE',
'Maximum model space distance between geometric entities at asserted c
onnectivities');
#23563=UNCERTAINTY_MEASURE_WITH_UNIT(LENGTH_MEASURE(0.01),#23578,
'DISTANCE_ACCURACY_VALUE',
'Maximum model space distance between geometric entities at asserted c
onnectivities');
#23564=UNCERTAINTY_MEASURE_WITH_UNIT(LENGTH_MEASURE(0.01),#23578,
'DISTANCE_ACCURACY_VALUE',
'Maximum model space distance between geometric entities at asserted c
onnectivities');
#23565=UNCERTAINTY_MEASURE_WITH_UNIT(LENGTH_MEASURE(0.01),#23578,
'DISTANCE_ACCURACY_VALUE',
'Maximum model space distance between geometric entities at asserted c
onnectivities');
#23566=UNCERTAINTY_MEASURE_WITH_UNIT(LENGTH_MEASURE(0.01),#23578,
'DISTANCE_ACCURACY_VALUE',
'Maximum model space distance between geometric entities at asserted c
onnectivities');
#23567=(
GEOMETRIC_REPRESENTATION_CONTEXT(3)
GLOBAL_UNCERTAINTY_ASSIGNED_CONTEXT((#23556))
GLOBAL_UNIT_ASSIGNED_CONTEXT((#23578,#23580,#23581))
REPRESENTATION_CONTEXT('','3D')
);
#23568=(
GEOMETRIC_REPRESENTATION_CONTEXT(3)
GLOBAL_UNCERTAINTY_ASSIGNED_CONTEXT((#23557))
GLOBAL_UNIT_ASSIGNED_CONTEXT((#23578,#23580,#23581))
REPRESENTATION_CONTEXT('','3D')
);
#23569=(
GEOMETRIC_REPRESENTATION_CONTEXT(3)
GLOBAL_UNCERTAINTY_ASSIGNED_CONTEXT((#23558))
GLOBAL_UNIT_ASSIGNED_CONTEXT((#23578,#23580,#23581))
REPRESENTATION_CONTEXT('','3D')
);
#23570=(
GEOMETRIC_REPRESENTATION_CONTEXT(3)
GLOBAL_UNCERTAINTY_ASSIGNED_CONTEXT((#23559))
GLOBAL_UNIT_ASSIGNED_CONTEXT((#23578,#23580,#23581))
REPRESENTATION_CONTEXT('','3D')
);
#23571=(
GEOMETRIC_REPRESENTATION_CONTEXT(3)
GLOBAL_UNCERTAINTY_ASSIGNED_CONTEXT((#23560))
GLOBAL_UNIT_ASSIGNED_CONTEXT((#23578,#23580,#23581))
REPRESENTATION_CONTEXT('','3D')
);
#23572=(
GEOMETRIC_REPRESENTATION_CONTEXT(3)
GLOBAL_UNCERTAINTY_ASSIGNED_CONTEXT((#23561))
GLOBAL_UNIT_ASSIGNED_CONTEXT((#23578,#23580,#23581))
REPRESENTATION_CONTEXT('','3D')
);
#23573=(
GEOMETRIC_REPRESENTATION_CONTEXT(3)
GLOBAL_UNCERTAINTY_ASSIGNED_CONTEXT((#23562))
GLOBAL_UNIT_ASSIGNED_CONTEXT((#23578,#23580,#23581))
REPRESENTATION_CONTEXT('','3D')
);
#23574=(
GEOMETRIC_REPRESENTATION_CONTEXT(3)
GLOBAL_UNCERTAINTY_ASSIGNED_CONTEXT((#23563))
GLOBAL_UNIT_ASSIGNED_CONTEXT((#23578,#23580,#23581))
REPRESENTATION_CONTEXT('','3D')
);
#23575=(
GEOMETRIC_REPRESENTATION_CONTEXT(3)
GLOBAL_UNCERTAINTY_ASSIGNED_CONTEXT((#23564))
GLOBAL_UNIT_ASSIGNED_CONTEXT((#23578,#23580,#23581))
REPRESENTATION_CONTEXT('','3D')
);
#23576=(
GEOMETRIC_REPRESENTATION_CONTEXT(3)
GLOBAL_UNCERTAINTY_ASSIGNED_CONTEXT((#23565))
GLOBAL_UNIT_ASSIGNED_CONTEXT((#23578,#23580,#23581))
REPRESENTATION_CONTEXT('','3D')
);
#23577=(
GEOMETRIC_REPRESENTATION_CONTEXT(3)
GLOBAL_UNCERTAINTY_ASSIGNED_CONTEXT((#23566))
GLOBAL_UNIT_ASSIGNED_CONTEXT((#23578,#23580,#23581))
REPRESENTATION_CONTEXT('','3D')
);
#23578=(
LENGTH_UNIT()
NAMED_UNIT(*)
SI_UNIT(.MILLI.,.METRE.)
);
#23579=(
LENGTH_UNIT()
NAMED_UNIT(*)
SI_UNIT($,.METRE.)
);
#23580=(
NAMED_UNIT(*)
PLANE_ANGLE_UNIT()
SI_UNIT($,.RADIAN.)
);
#23581=(
NAMED_UNIT(*)
SI_UNIT($,.STERADIAN.)
SOLID_ANGLE_UNIT()
);
#23582=SHAPE_DEFINITION_REPRESENTATION(#23592,#23611);
#23583=SHAPE_DEFINITION_REPRESENTATION(#23593,#23612);
#23584=SHAPE_DEFINITION_REPRESENTATION(#23594,#23613);
#23585=SHAPE_DEFINITION_REPRESENTATION(#23595,#23614);
#23586=SHAPE_DEFINITION_REPRESENTATION(#23596,#23615);
#23587=SHAPE_DEFINITION_REPRESENTATION(#23597,#23616);
#23588=SHAPE_DEFINITION_REPRESENTATION(#23598,#23617);
#23589=SHAPE_DEFINITION_REPRESENTATION(#23599,#23618);
#23590=SHAPE_DEFINITION_REPRESENTATION(#23600,#23619);
#23591=SHAPE_DEFINITION_REPRESENTATION(#23601,#23620);
#23592=PRODUCT_DEFINITION_SHAPE('',$,#23622);
#23593=PRODUCT_DEFINITION_SHAPE('',$,#23623);
#23594=PRODUCT_DEFINITION_SHAPE('',$,#23624);
#23595=PRODUCT_DEFINITION_SHAPE('',$,#23625);
#23596=PRODUCT_DEFINITION_SHAPE('',$,#23626);
#23597=PRODUCT_DEFINITION_SHAPE('',$,#23627);
#23598=PRODUCT_DEFINITION_SHAPE('',$,#23628);
#23599=PRODUCT_DEFINITION_SHAPE('',$,#23629);
#23600=PRODUCT_DEFINITION_SHAPE('',$,#23630);
#23601=PRODUCT_DEFINITION_SHAPE('',$,#23631);
#23602=PRODUCT_DEFINITION_SHAPE($,$,#38);
#23603=PRODUCT_DEFINITION_SHAPE($,$,#39);
#23604=PRODUCT_DEFINITION_SHAPE($,$,#40);
#23605=PRODUCT_DEFINITION_SHAPE($,$,#41);
#23606=PRODUCT_DEFINITION_SHAPE($,$,#42);
#23607=PRODUCT_DEFINITION_SHAPE($,$,#43);
#23608=PRODUCT_DEFINITION_SHAPE($,$,#44);
#23609=PRODUCT_DEFINITION_SHAPE($,$,#45);
#23610=PRODUCT_DEFINITION_SHAPE($,$,#46);
#23611=SHAPE_REPRESENTATION('',(#4266,#4665,#4666,#4667,#4668,#4669,#4670,
#4671,#4672,#4673),#23567);
#23612=SHAPE_REPRESENTATION('',(#4267),#23568);
#23613=SHAPE_REPRESENTATION('',(#4284),#23569);
#23614=SHAPE_REPRESENTATION('',(#4354),#23570);
#23615=SHAPE_REPRESENTATION('',(#4424),#23571);
#23616=SHAPE_REPRESENTATION('',(#4436),#23572);
#23617=SHAPE_REPRESENTATION('',(#4473),#23573);
#23618=SHAPE_REPRESENTATION('',(#4485),#23574);
#23619=SHAPE_REPRESENTATION('',(#4573),#23575);
#23620=SHAPE_REPRESENTATION('',(#4607),#23576);
#23621=PRODUCT_DEFINITION_CONTEXT('part definition',#23653,'design');
#23622=PRODUCT_DEFINITION('BR-203','BR-203',#23632,#23621);
#23623=PRODUCT_DEFINITION('Clamp_03','Clamp_03',#23633,#23621);
#23624=PRODUCT_DEFINITION('Base_Left','Base_Left',#23634,#23621);
#23625=PRODUCT_DEFINITION('Base_Right','Base_Right',#23635,#23621);
#23626=PRODUCT_DEFINITION('Nut_01','Nut_01',#23636,#23621);
#23627=PRODUCT_DEFINITION('Screw','Screw',#23637,#23621);
#23628=PRODUCT_DEFINITION('Nut_02','Nut_02',#23638,#23621);
#23629=PRODUCT_DEFINITION('Clamp_01','Clamp_01',#23639,#23621);
#23630=PRODUCT_DEFINITION('Clamp_02','Clamp_02',#23640,#23621);
#23631=PRODUCT_DEFINITION('Cover','Cover',#23641,#23621);
#23632=PRODUCT_DEFINITION_FORMATION('',$,#23655);
#23633=PRODUCT_DEFINITION_FORMATION('',$,#23656);
#23634=PRODUCT_DEFINITION_FORMATION('',$,#23657);
#23635=PRODUCT_DEFINITION_FORMATION('',$,#23658);
#23636=PRODUCT_DEFINITION_FORMATION('',$,#23659);
#23637=PRODUCT_DEFINITION_FORMATION('',$,#23660);
#23638=PRODUCT_DEFINITION_FORMATION('',$,#23661);
#23639=PRODUCT_DEFINITION_FORMATION('',$,#23662);
#23640=PRODUCT_DEFINITION_FORMATION('',$,#23663);
#23641=PRODUCT_DEFINITION_FORMATION('',$,#23664);
#23642=PRODUCT_RELATED_PRODUCT_CATEGORY('BR-203','BR-203',(#23655));
#23643=PRODUCT_RELATED_PRODUCT_CATEGORY('Clamp_03','Clamp_03',(#23656));
#23644=PRODUCT_RELATED_PRODUCT_CATEGORY('Base_Left','Base_Left',(#23657));
#23645=PRODUCT_RELATED_PRODUCT_CATEGORY('Base_Right','Base_Right',(#23658));
#23646=PRODUCT_RELATED_PRODUCT_CATEGORY('Nut_01','Nut_01',(#23659));
#23647=PRODUCT_RELATED_PRODUCT_CATEGORY('Screw','Screw',(#23660));
#23648=PRODUCT_RELATED_PRODUCT_CATEGORY('Nut_02','Nut_02',(#23661));
#23649=PRODUCT_RELATED_PRODUCT_CATEGORY('Clamp_01','Clamp_01',(#23662));
#23650=PRODUCT_RELATED_PRODUCT_CATEGORY('Clamp_02','Clamp_02',(#23663));
#23651=PRODUCT_RELATED_PRODUCT_CATEGORY('Cover','Cover',(#23664));
#23652=APPLICATION_PROTOCOL_DEFINITION('international standard',
'automotive_design',2009,#23653);
#23653=APPLICATION_CONTEXT(
'Core Data for Automotive Mechanical Design Process');
#23654=PRODUCT_CONTEXT('part definition',#23653,'mechanical');
#23655=PRODUCT('BR-203','BR-203',$,(#23654));
#23656=PRODUCT('Clamp_03','Clamp_03',$,(#23654));
#23657=PRODUCT('Base_Left','Base_Left',$,(#23654));
#23658=PRODUCT('Base_Right','Base_Right',$,(#23654));
#23659=PRODUCT('Nut_01','Nut_01',$,(#23654));
#23660=PRODUCT('Screw','Screw',$,(#23654));
#23661=PRODUCT('Nut_02','Nut_02',$,(#23654));
#23662=PRODUCT('Clamp_01','Clamp_01',$,(#23654));
#23663=PRODUCT('Clamp_02','Clamp_02',$,(#23654));
#23664=PRODUCT('Cover','Cover',$,(#23654));
#23665=PRESENTATION_STYLE_ASSIGNMENT((#23670));
#23666=PRESENTATION_STYLE_ASSIGNMENT((#23671));
#23667=PRESENTATION_STYLE_ASSIGNMENT((#23672));
#23668=PRESENTATION_STYLE_ASSIGNMENT((#23673));
#23669=PRESENTATION_STYLE_ASSIGNMENT((#23674));
#23670=SURFACE_STYLE_USAGE(.BOTH.,#23675);
#23671=SURFACE_STYLE_USAGE(.BOTH.,#23676);
#23672=SURFACE_STYLE_USAGE(.BOTH.,#23677);
#23673=SURFACE_STYLE_USAGE(.BOTH.,#23678);
#23674=SURFACE_STYLE_USAGE(.BOTH.,#23679);
#23675=SURFACE_SIDE_STYLE('',(#23680));
#23676=SURFACE_SIDE_STYLE('',(#23681));
#23677=SURFACE_SIDE_STYLE('',(#23682));
#23678=SURFACE_SIDE_STYLE('',(#23683));
#23679=SURFACE_SIDE_STYLE('',(#23684));
#23680=SURFACE_STYLE_FILL_AREA(#23685);
#23681=SURFACE_STYLE_FILL_AREA(#23686);
#23682=SURFACE_STYLE_FILL_AREA(#23687);
#23683=SURFACE_STYLE_FILL_AREA(#23688);
#23684=SURFACE_STYLE_FILL_AREA(#23689);
#23685=FILL_AREA_STYLE('Steel - Satin',(#23690));
#23686=FILL_AREA_STYLE('Opaque(210,210,210)',(#23691));
#23687=FILL_AREA_STYLE('Opaque(151,151,151)',(#23692));
#23688=FILL_AREA_STYLE('Opaque(222,222,222)',(#23693));
#23689=FILL_AREA_STYLE('Opaque(144,209,199)',(#23694));
#23690=FILL_AREA_STYLE_COLOUR('Steel - Satin',#23695);
#23691=FILL_AREA_STYLE_COLOUR('Opaque(210,210,210)',#23696);
#23692=FILL_AREA_STYLE_COLOUR('Opaque(151,151,151)',#23697);
#23693=FILL_AREA_STYLE_COLOUR('Opaque(222,222,222)',#23698);
#23694=FILL_AREA_STYLE_COLOUR('Opaque(144,209,199)',#23699);
#23695=COLOUR_RGB('Steel - Satin', 0.09019608, 0.27058824, 0.51372549);
#23696=COLOUR_RGB('Opaque(210,210,210)', 0.09019608, 0.27058824, 0.51372549);
#23697=COLOUR_RGB('Opaque(151,151,151)', 0.72549020, 0.75294118, 0.79215686);
#23698=COLOUR_RGB('Opaque(222,222,222)', 0.09019608, 0.27058824, 0.51372549);
#23699=COLOUR_RGB('Opaque(144,209,199)', 0.31764706, 0.68627451, 0.89019608);
ENDSEC;
END-ISO-10303-21;
